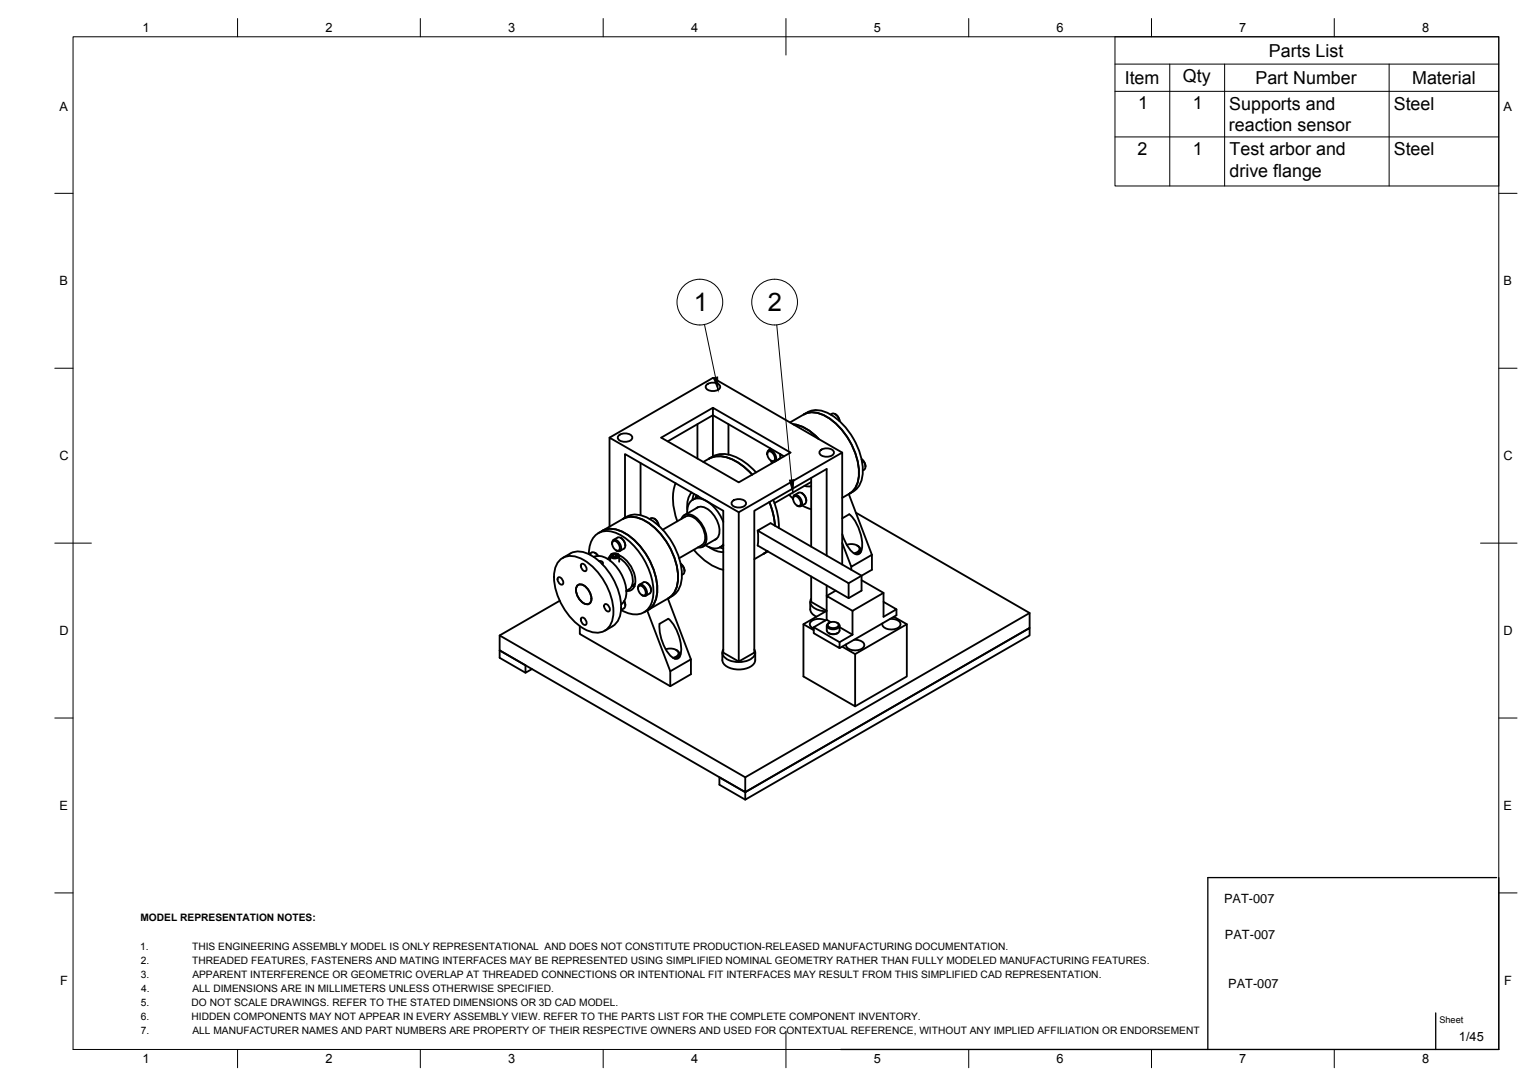
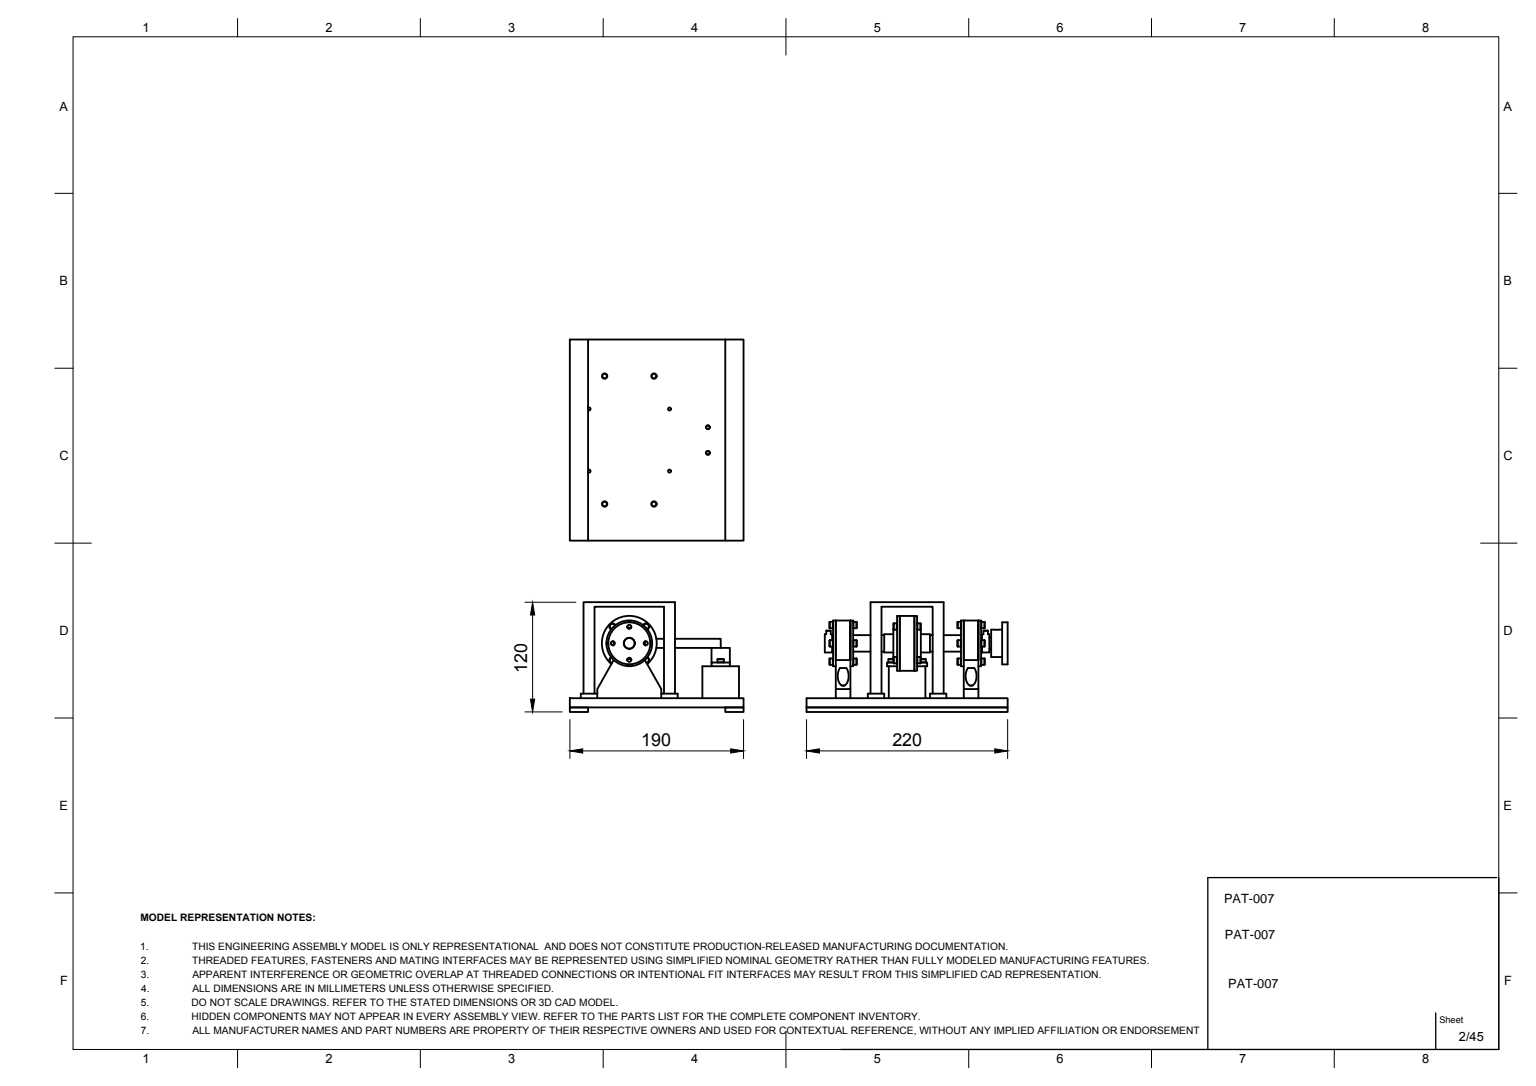
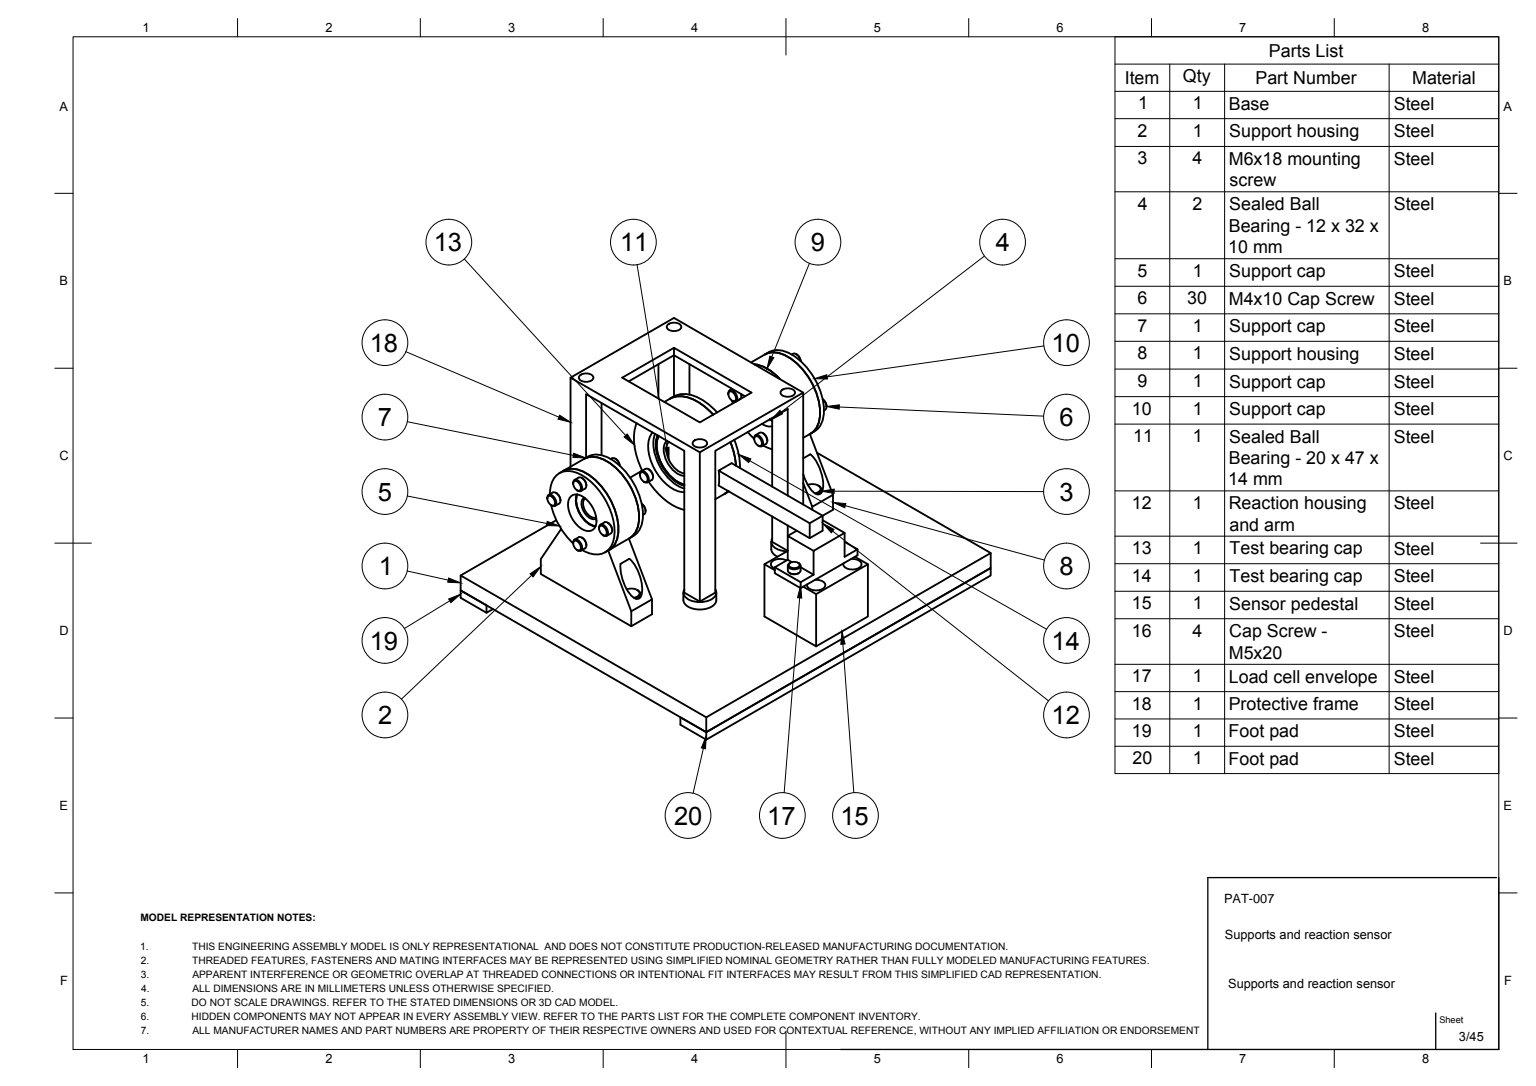
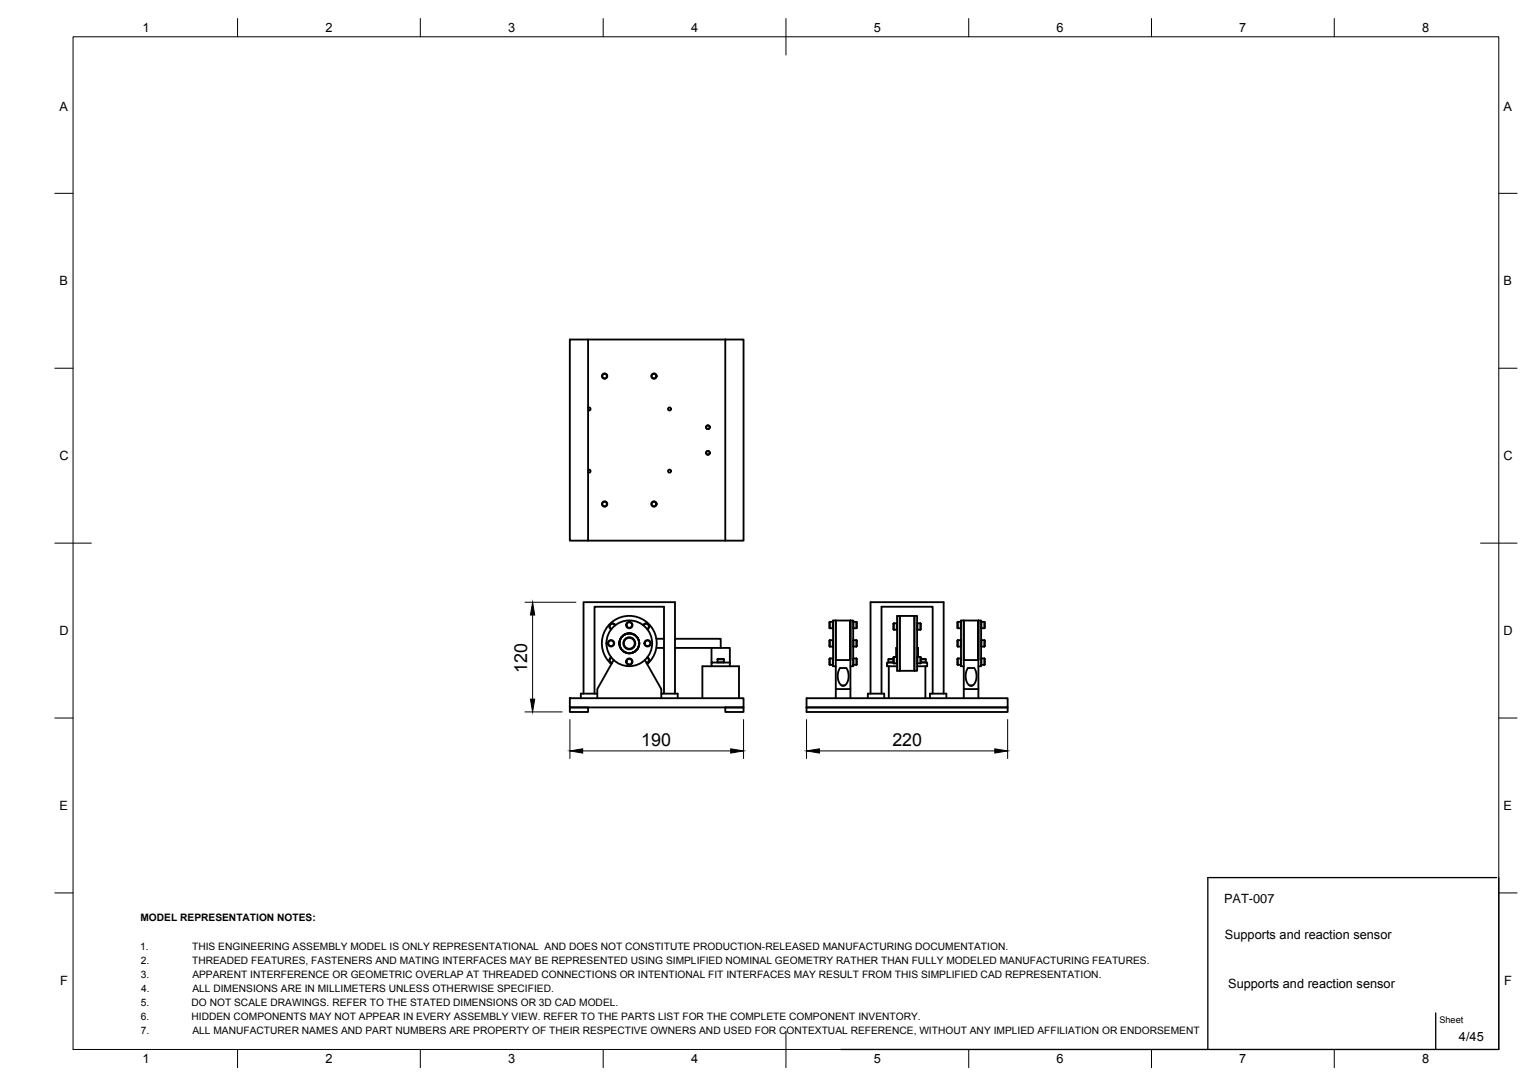
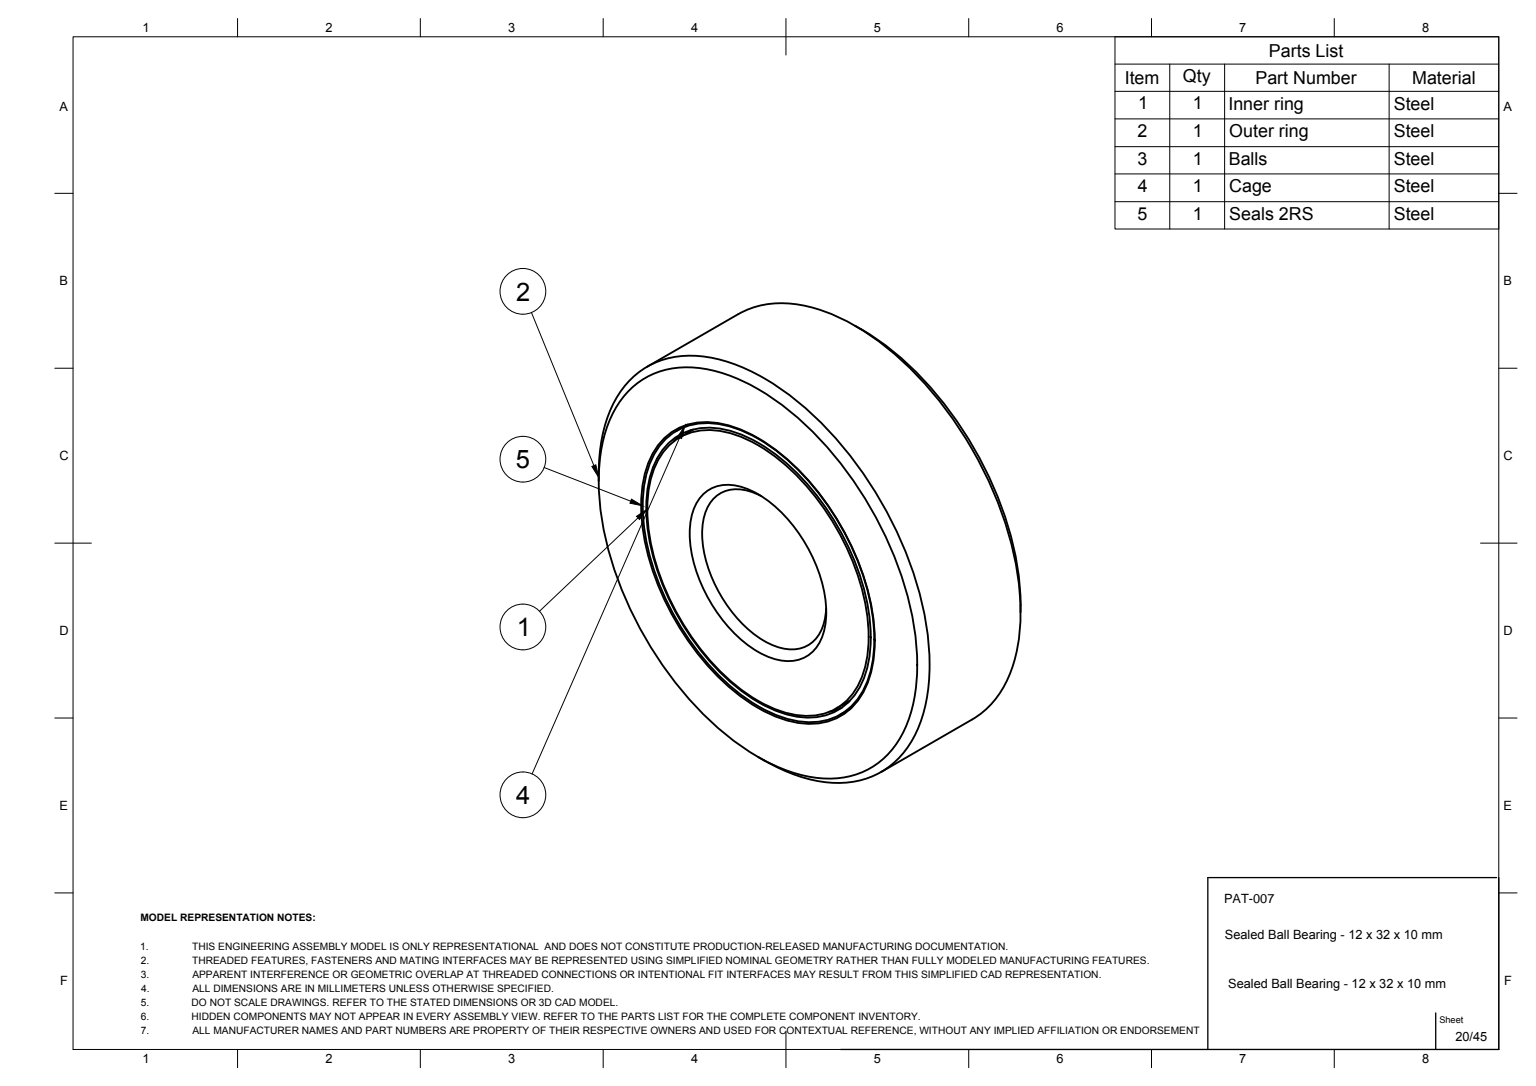
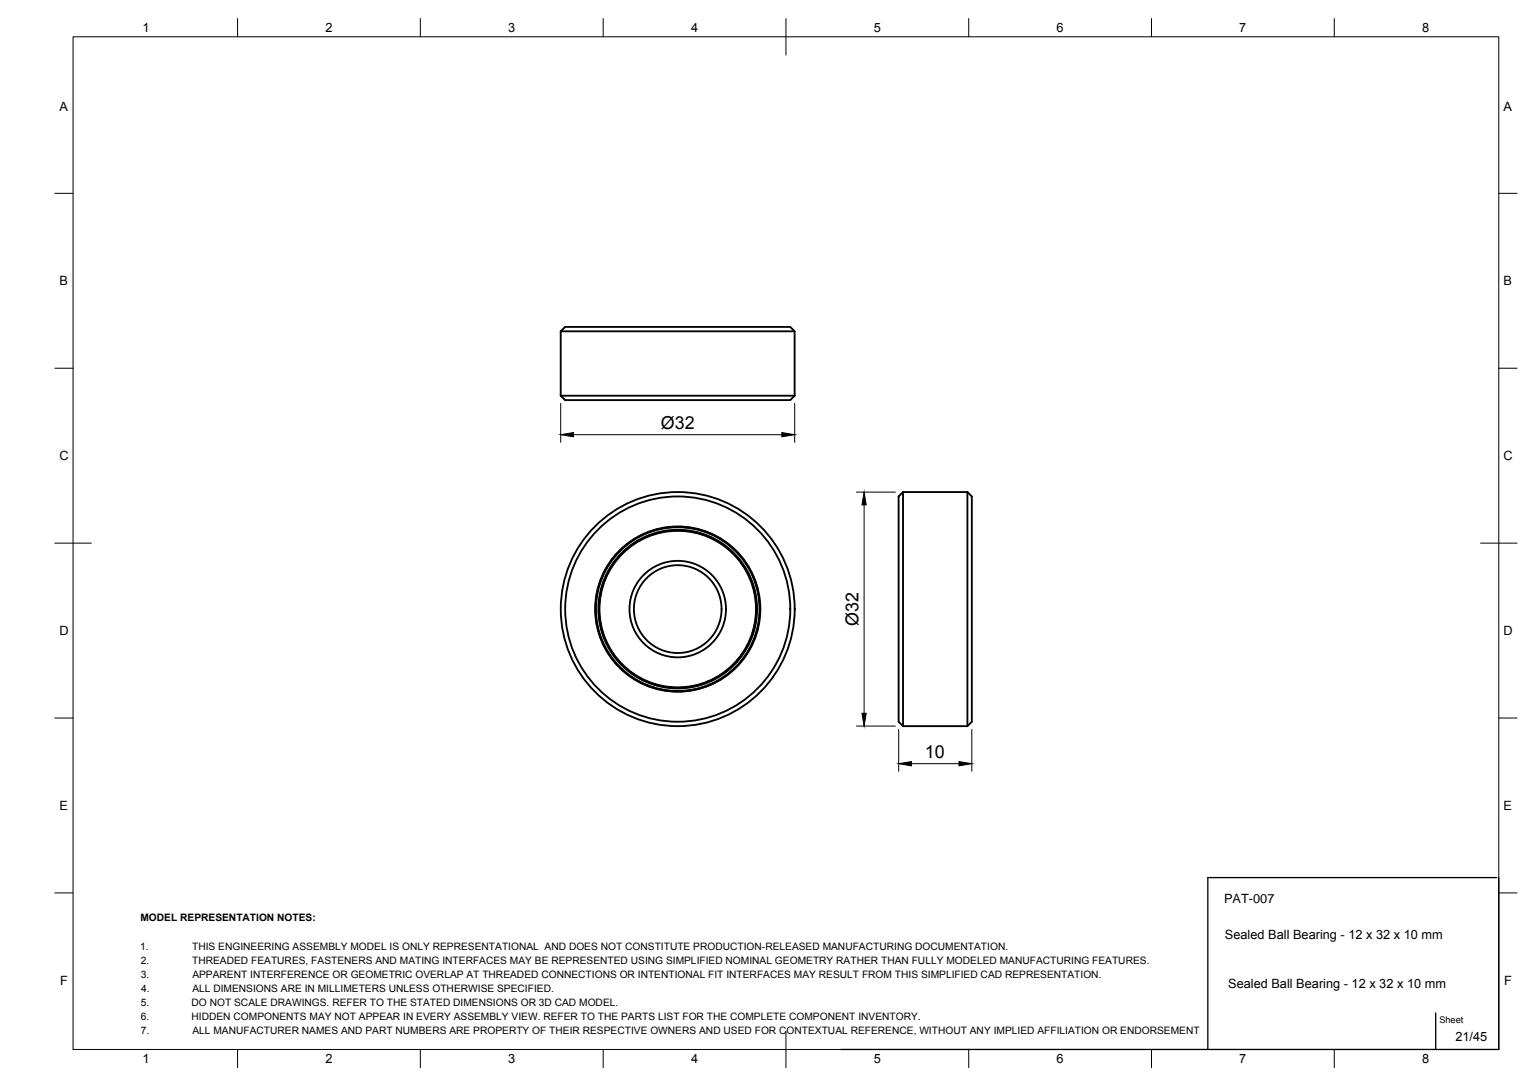
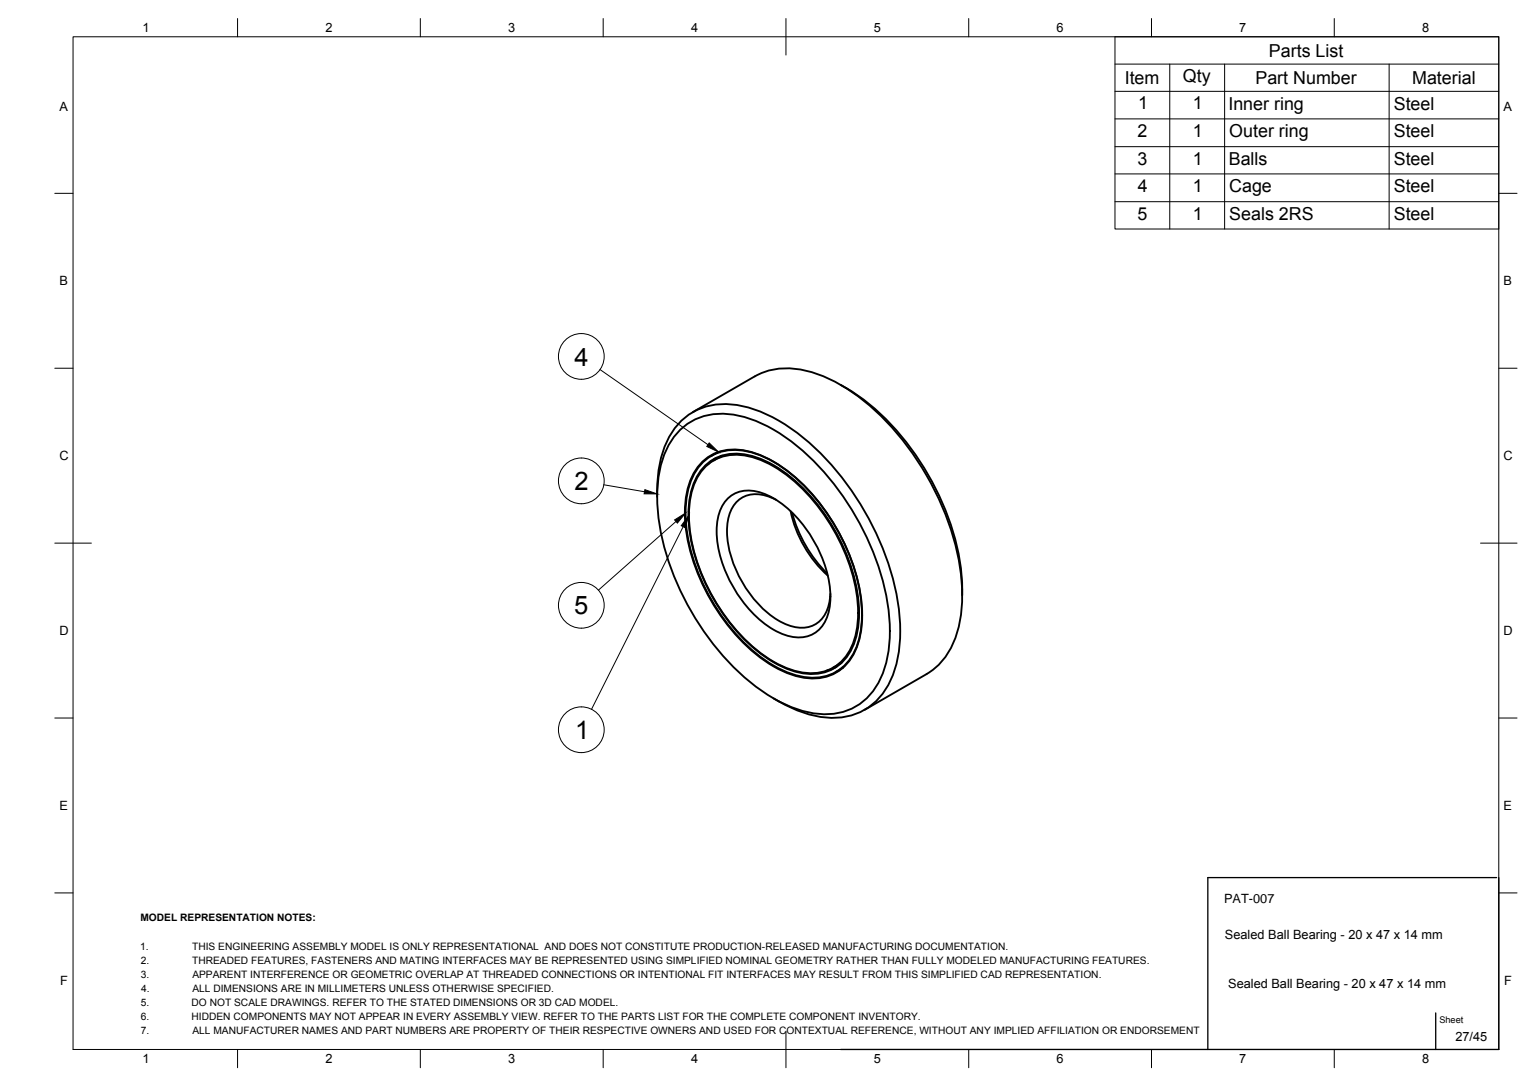
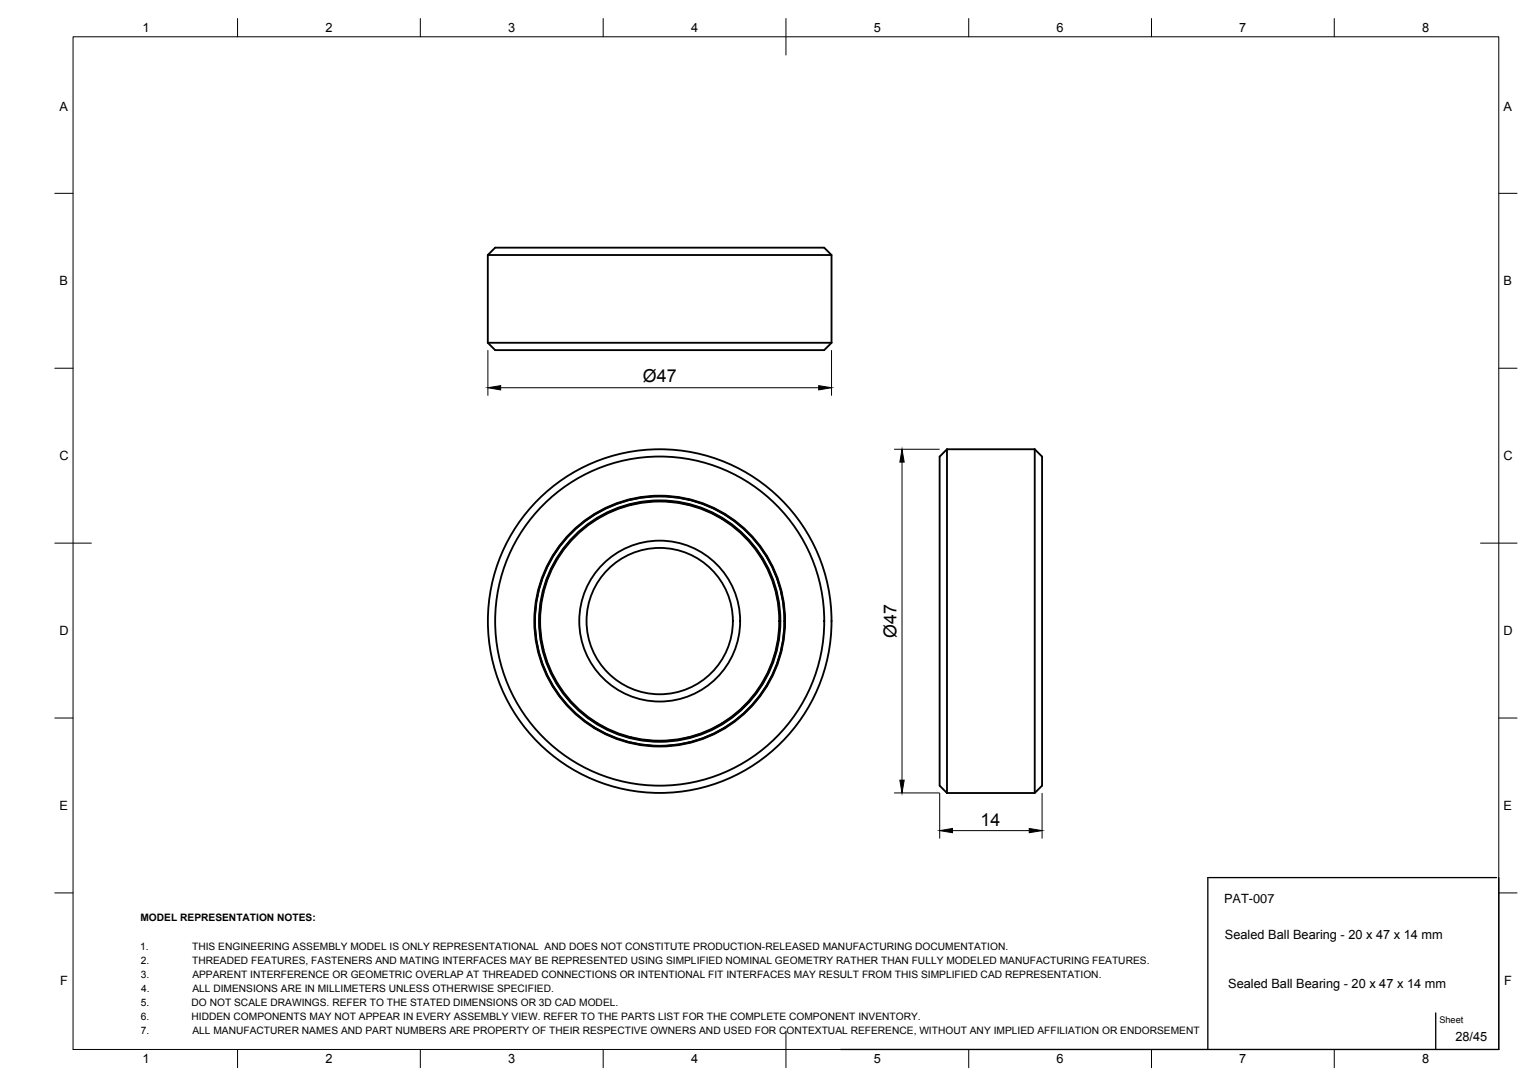
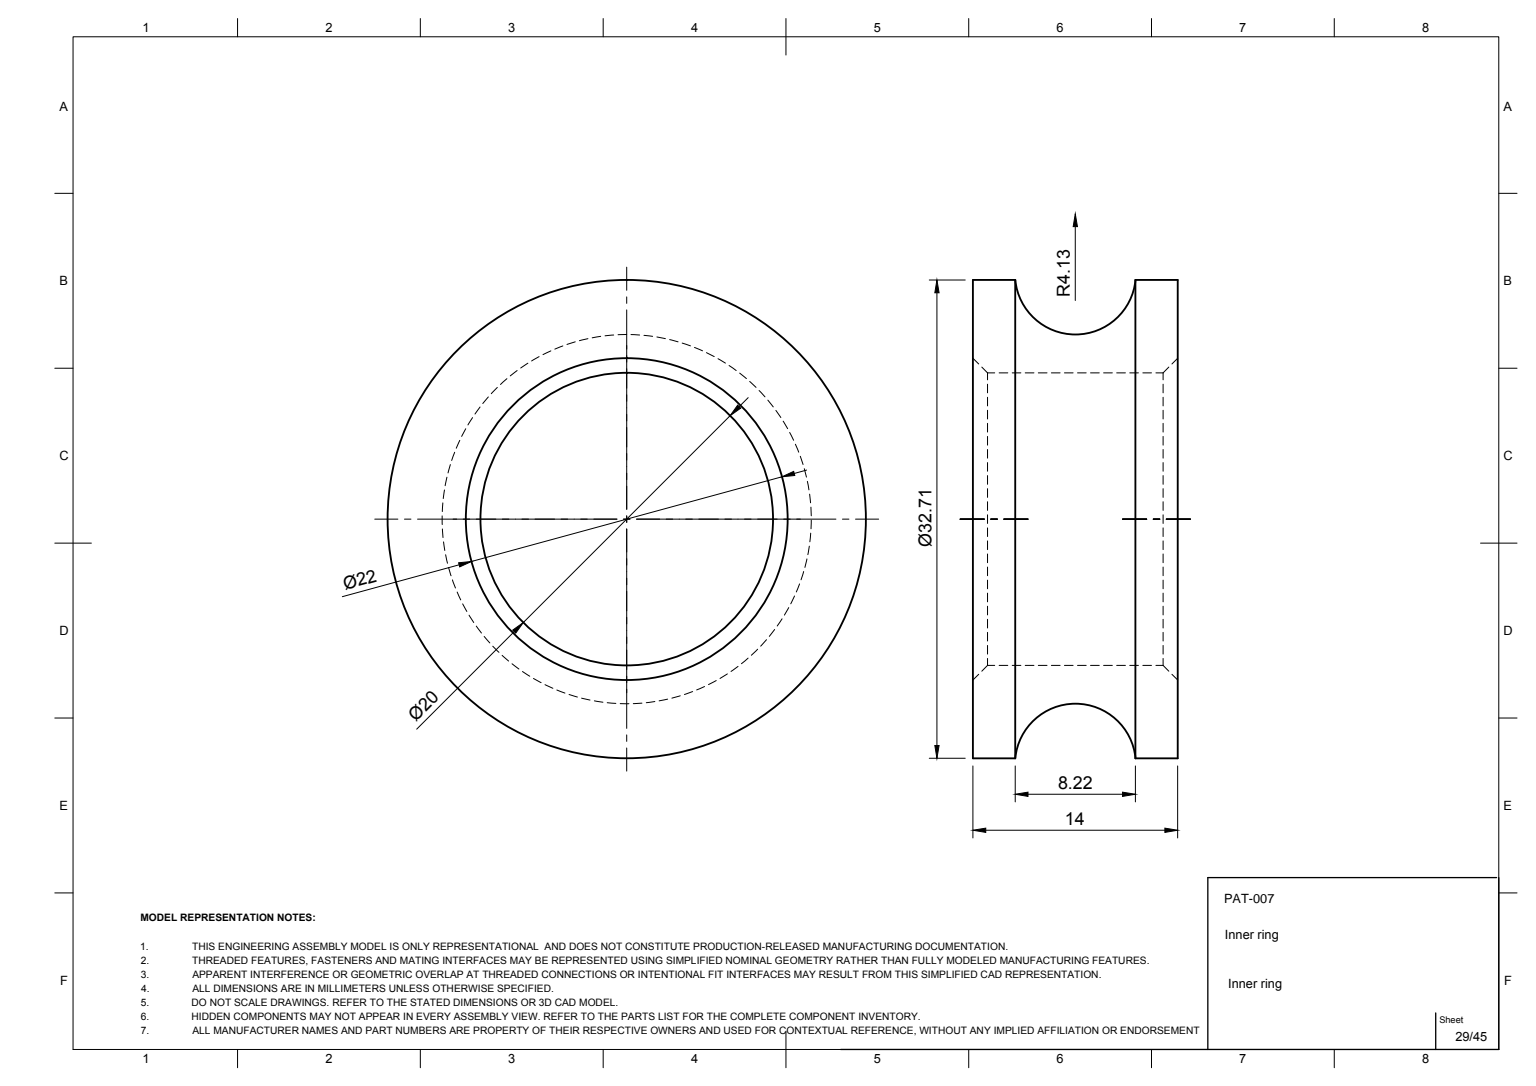
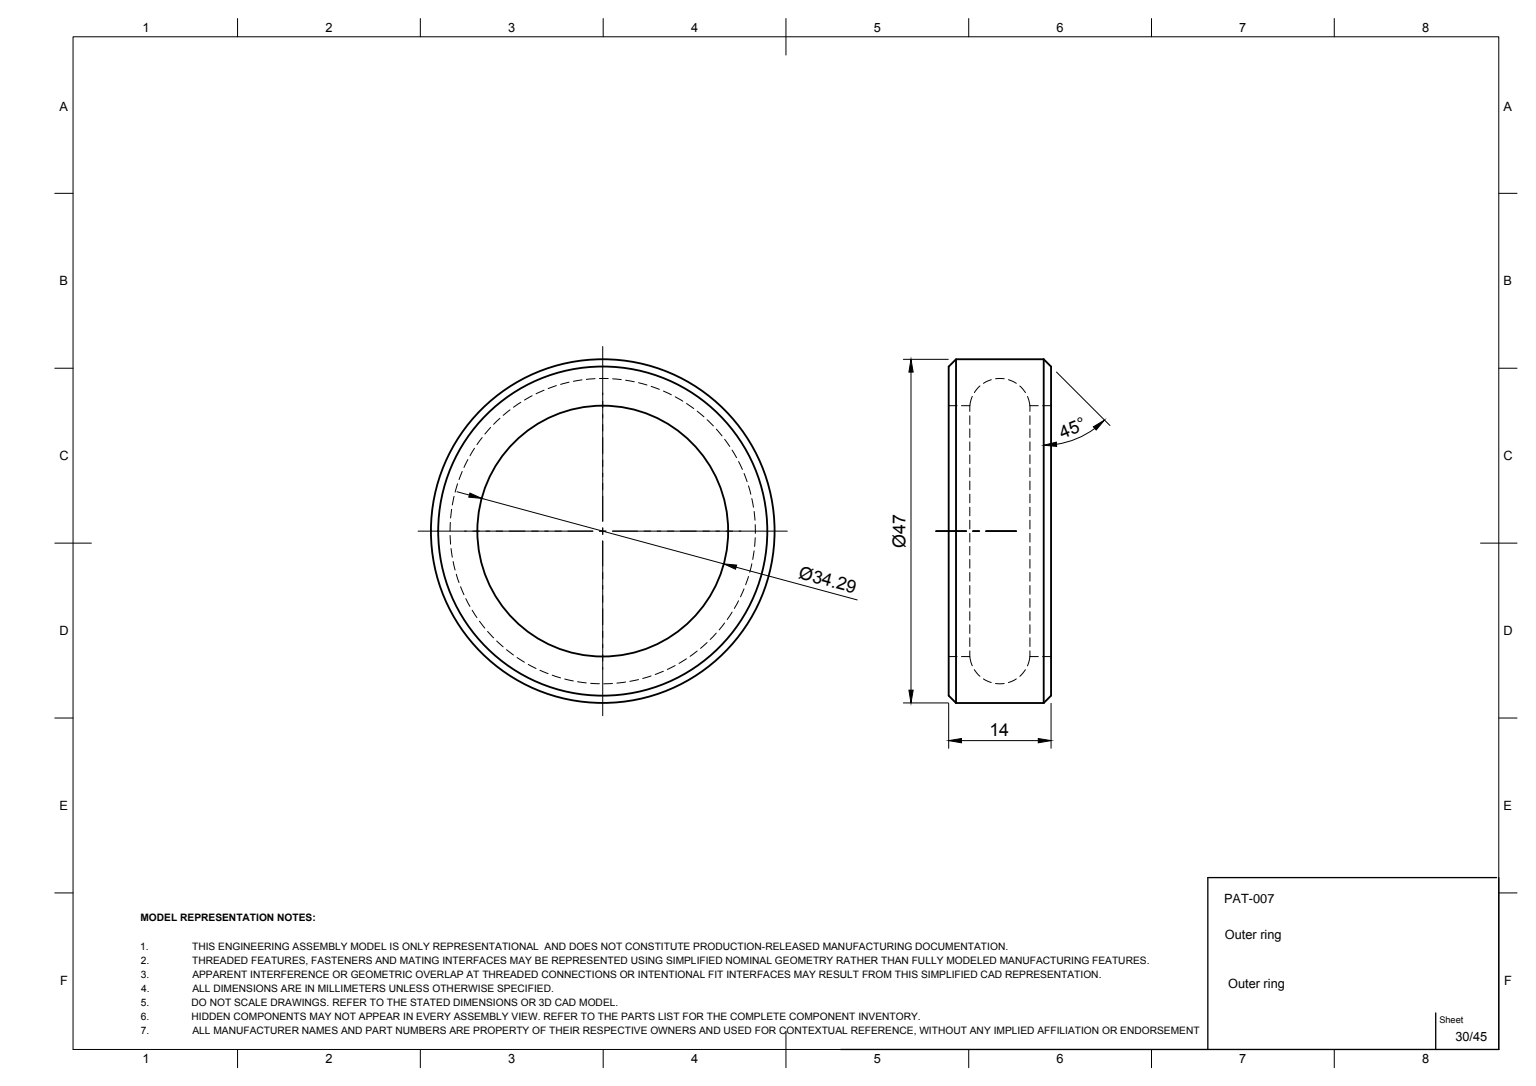
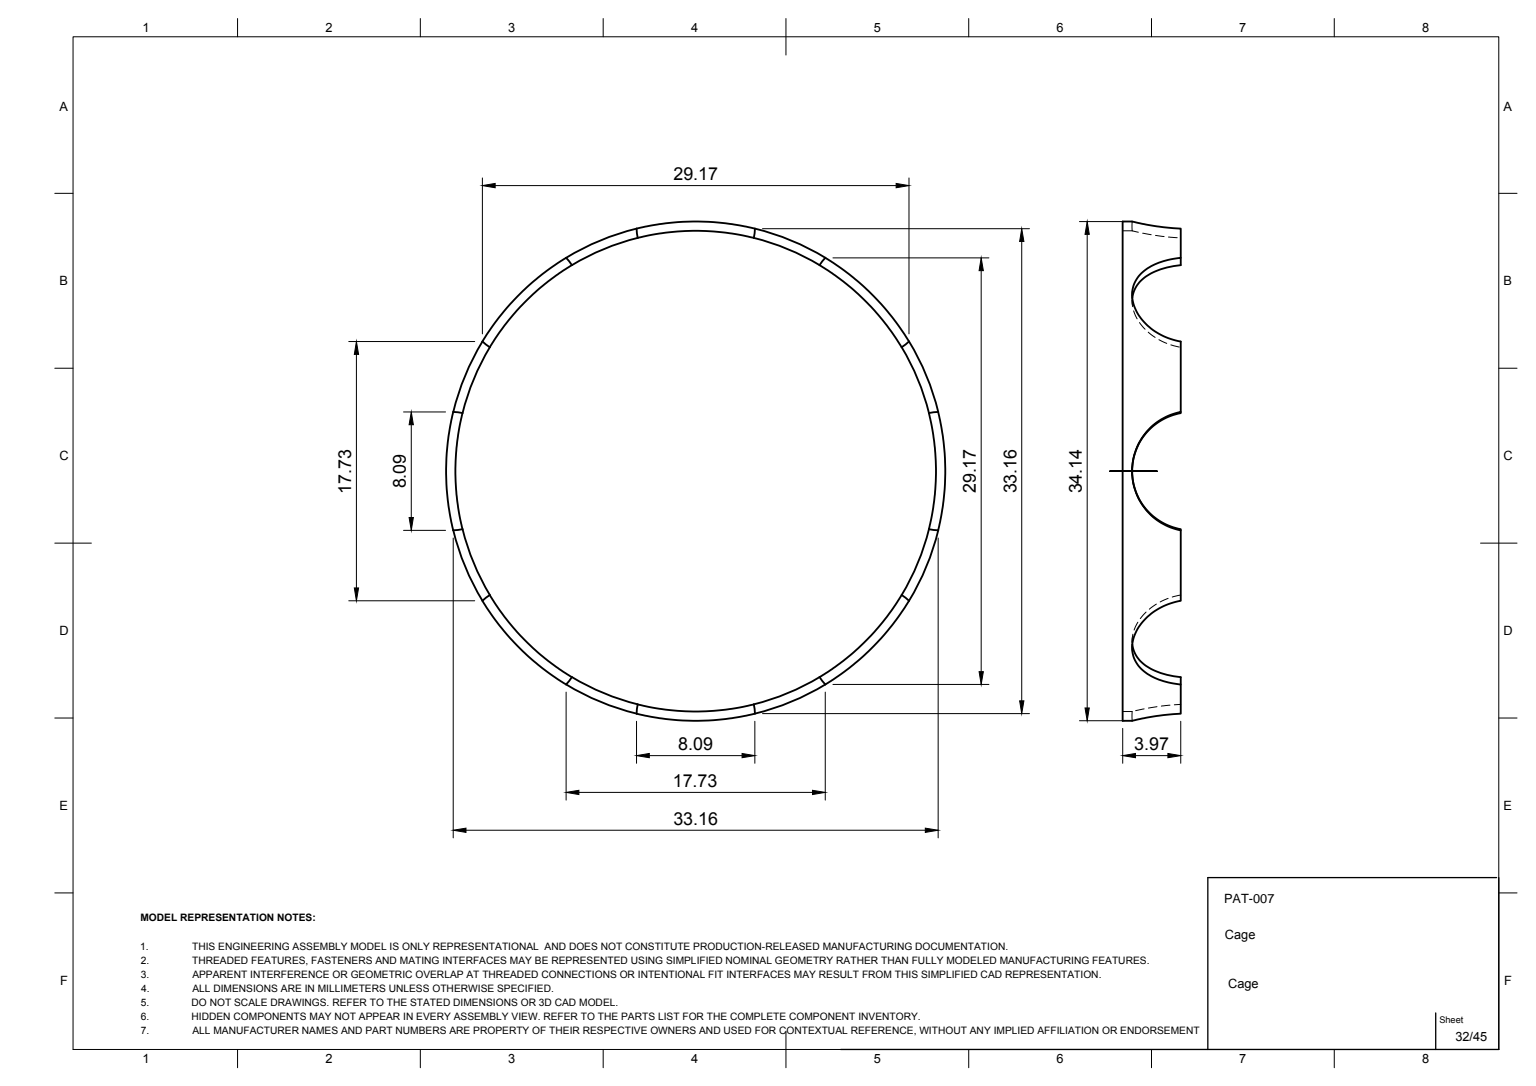
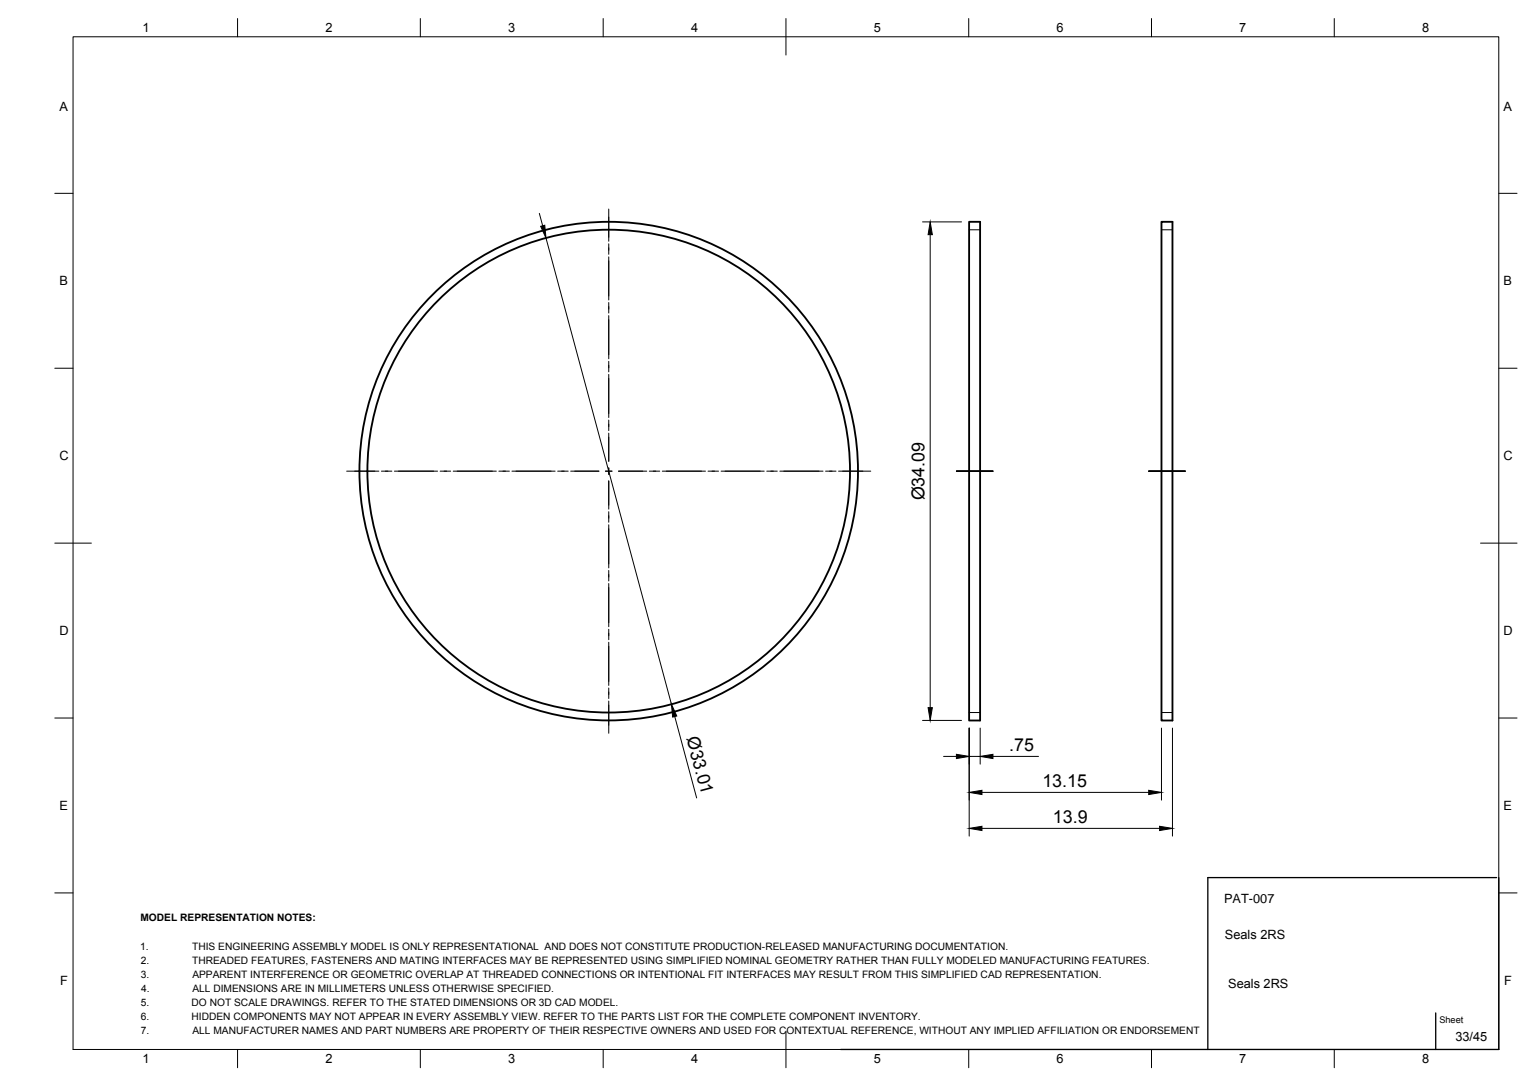
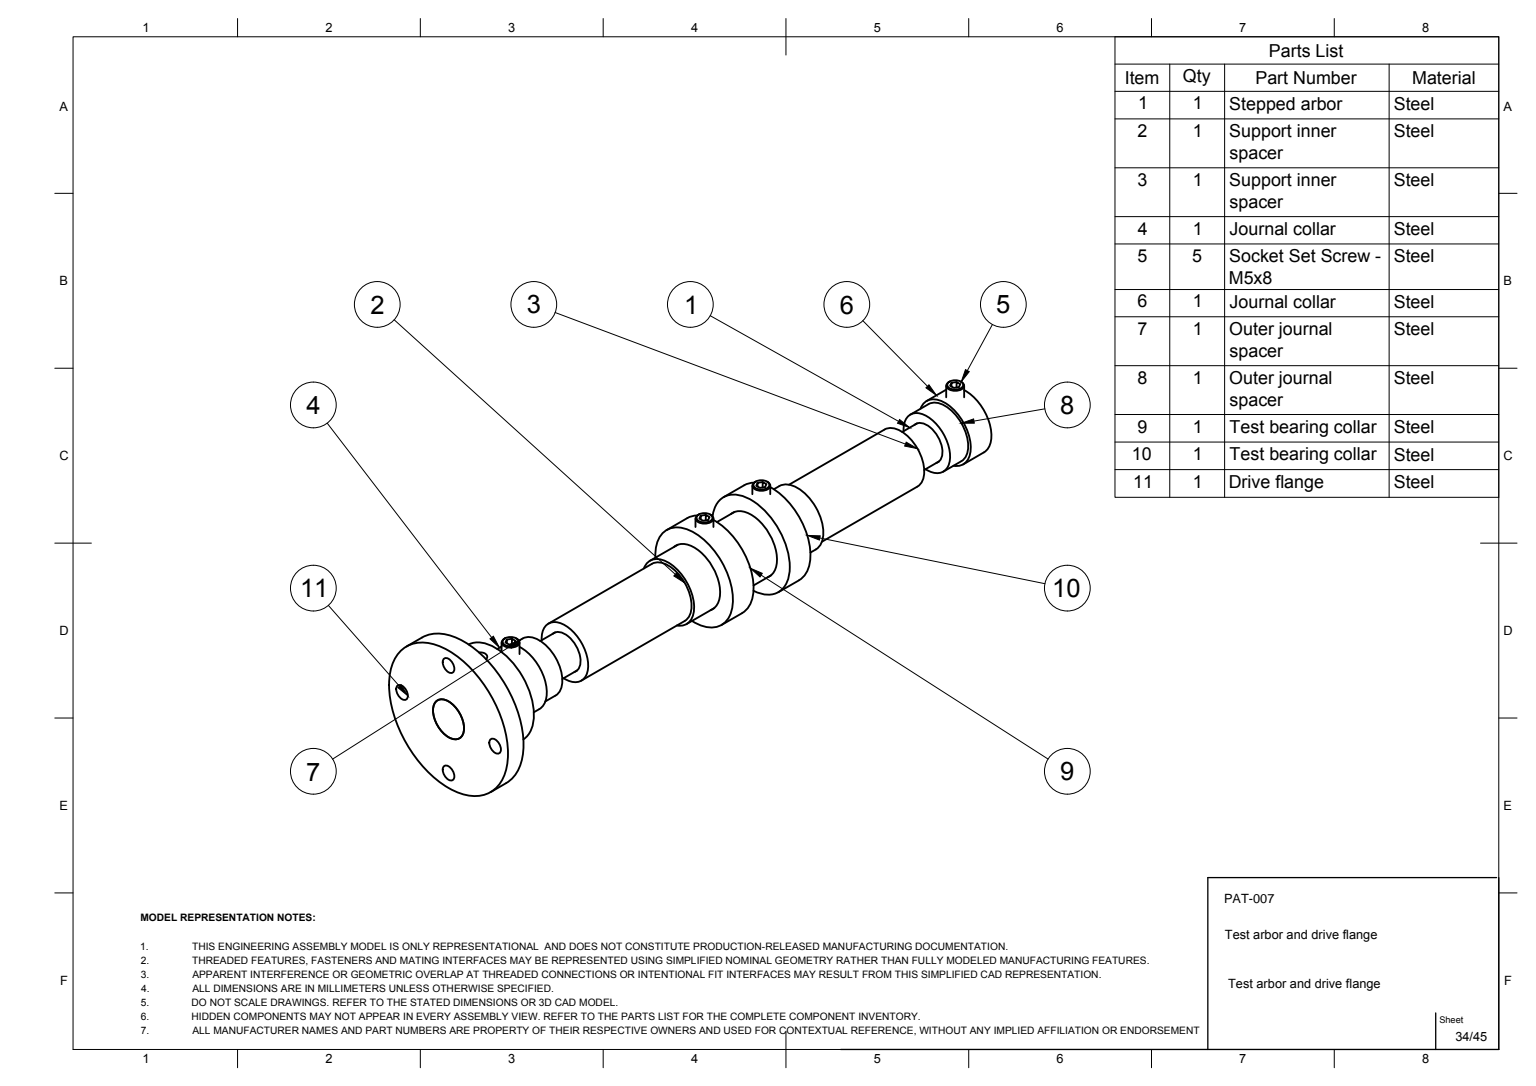
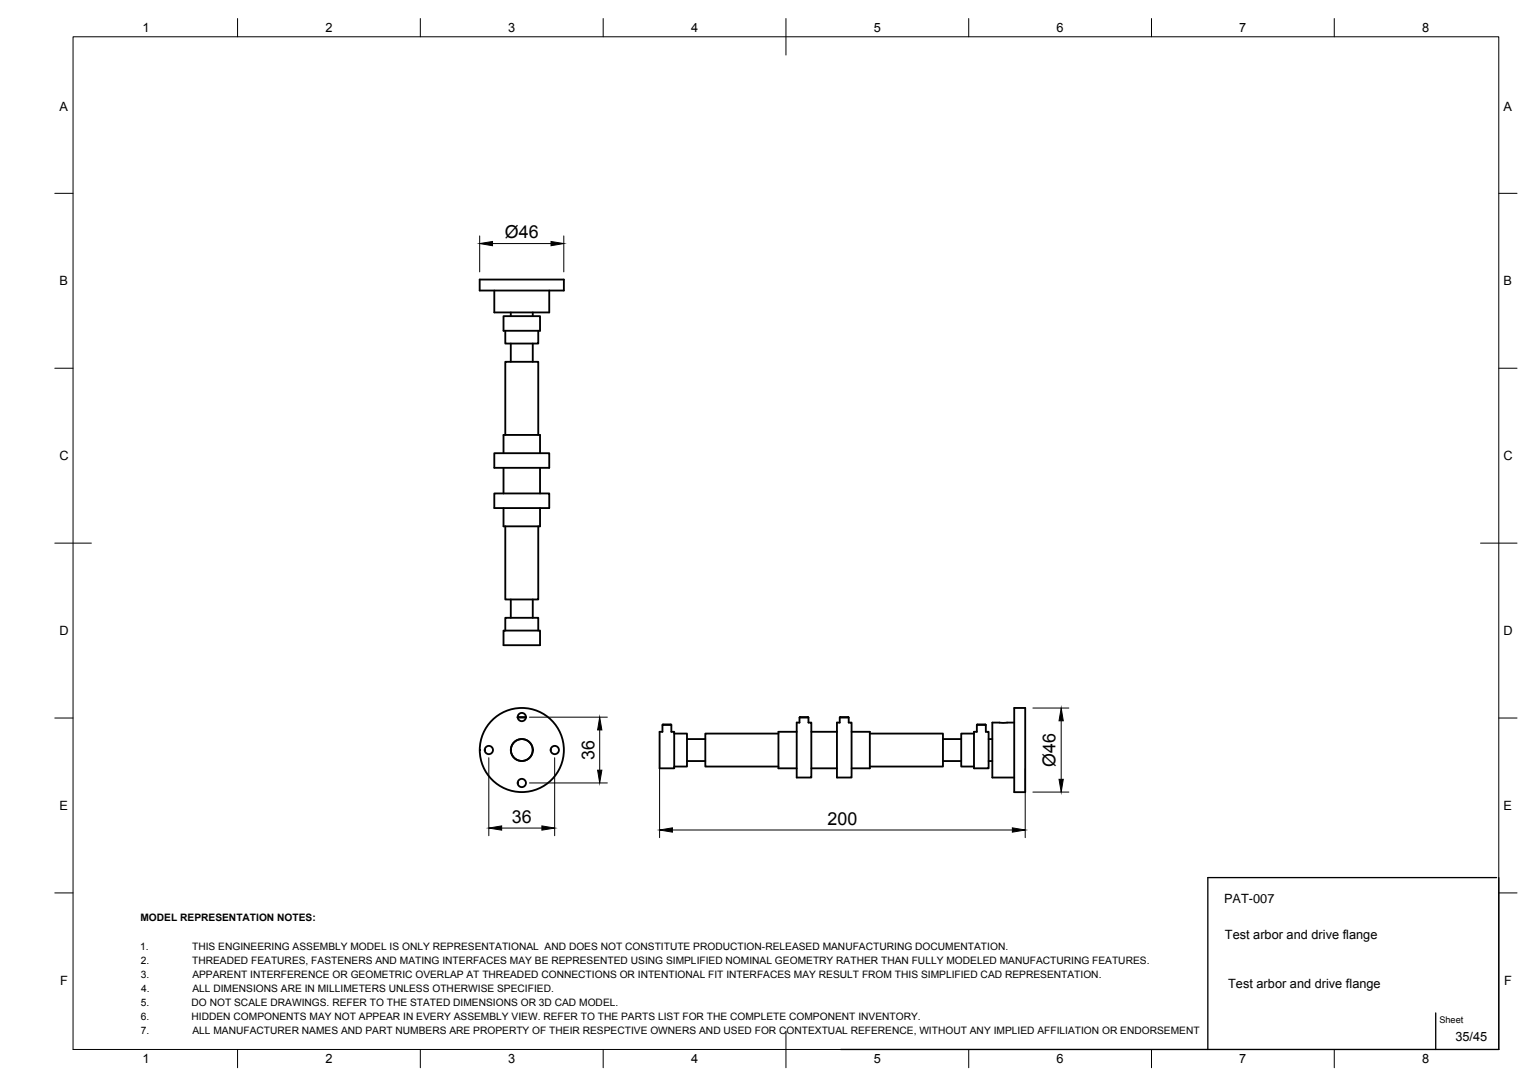
ISO-10303-21;
HEADER;
/* Generated by software containing ST-Developer
 * from STEP Tools, Inc. (www.steptools.com) 
 */

FILE_DESCRIPTION(
/* description */ ('Bearing friction torque test rig'),
/* implementation_level */ '2;1');

FILE_NAME(
/* name */ 'PAT-007',
/* time_stamp */ '2026-10-28T03:24:04-07:00',
/* author */ (''),
/* organization */ (''),
/* preprocessor_version */ 'ST-DEVELOPER v20.2',
/* originating_system */ 'Autodesk Translation Framework v15.17.0.0',
/* authorisation */ '');

FILE_SCHEMA (('AUTOMOTIVE_DESIGN { 1 0 10303 214 3 1 1 }'));
ENDSEC;

DATA;
#10=MECHANICAL_DESIGN_GEOMETRIC_PRESENTATION_REPRESENTATION('',(#539,#540,
#541,#542,#543,#544,#545,#546,#547,#548,#549,#550,#551,#552,#553,#554,#555,
#556,#557,#558,#559,#560,#561,#562,#563,#564,#565,#566,#567,#568,#569,#570,
#571,#572,#573,#574,#575,#576,#577,#578,#579,#580,#581,#582,#583,#584,#585,
#586,#587,#588,#589,#590,#591,#592),#14822);
#11=ITEM_DEFINED_TRANSFORMATION($,$,#8623,#8745);
#12=ITEM_DEFINED_TRANSFORMATION($,$,#8643,#8746);
#13=ITEM_DEFINED_TRANSFORMATION($,$,#8663,#8747);
#14=ITEM_DEFINED_TRANSFORMATION($,$,#8678,#8748);
#15=ITEM_DEFINED_TRANSFORMATION($,$,#8728,#8749);
#16=ITEM_DEFINED_TRANSFORMATION($,$,#8751,#8879);
#17=ITEM_DEFINED_TRANSFORMATION($,$,#8771,#8880);
#18=ITEM_DEFINED_TRANSFORMATION($,$,#8791,#8881);
#19=ITEM_DEFINED_TRANSFORMATION($,$,#8808,#8882);
#20=ITEM_DEFINED_TRANSFORMATION($,$,#8862,#8883);
#21=ITEM_DEFINED_TRANSFORMATION($,$,#8144,#8934);
#22=ITEM_DEFINED_TRANSFORMATION($,$,#8187,#8935);
#23=ITEM_DEFINED_TRANSFORMATION($,$,#8233,#8936);
#24=ITEM_DEFINED_TRANSFORMATION($,$,#8258,#8937);
#25=ITEM_DEFINED_TRANSFORMATION($,$,#8283,#8938);
#26=ITEM_DEFINED_TRANSFORMATION($,$,#8329,#8939);
#27=ITEM_DEFINED_TRANSFORMATION($,$,#8354,#8940);
#28=ITEM_DEFINED_TRANSFORMATION($,$,#8379,#8941);
#29=ITEM_DEFINED_TRANSFORMATION($,$,#8407,#8942);
#30=ITEM_DEFINED_TRANSFORMATION($,$,#8432,#8943);
#31=ITEM_DEFINED_TRANSFORMATION($,$,#8457,#8944);
#32=ITEM_DEFINED_TRANSFORMATION($,$,#8500,#8945);
#33=ITEM_DEFINED_TRANSFORMATION($,$,#8517,#8946);
#34=ITEM_DEFINED_TRANSFORMATION($,$,#8584,#8947);
#35=ITEM_DEFINED_TRANSFORMATION($,$,#8591,#8948);
#36=ITEM_DEFINED_TRANSFORMATION($,$,#8598,#8949);
#37=ITEM_DEFINED_TRANSFORMATION($,$,#8598,#8950);
#38=ITEM_DEFINED_TRANSFORMATION($,$,#8622,#8951);
#39=ITEM_DEFINED_TRANSFORMATION($,$,#8910,#8952);
#40=ITEM_DEFINED_TRANSFORMATION($,$,#8910,#8953);
#41=ITEM_DEFINED_TRANSFORMATION($,$,#8910,#8954);
#42=ITEM_DEFINED_TRANSFORMATION($,$,#8910,#8955);
#43=ITEM_DEFINED_TRANSFORMATION($,$,#8910,#8956);
#44=ITEM_DEFINED_TRANSFORMATION($,$,#8910,#8957);
#45=ITEM_DEFINED_TRANSFORMATION($,$,#8910,#8958);
#46=ITEM_DEFINED_TRANSFORMATION($,$,#8910,#8959);
#47=ITEM_DEFINED_TRANSFORMATION($,$,#8598,#8960);
#48=ITEM_DEFINED_TRANSFORMATION($,$,#8598,#8961);
#49=ITEM_DEFINED_TRANSFORMATION($,$,#8622,#8962);
#50=ITEM_DEFINED_TRANSFORMATION($,$,#8910,#8963);
#51=ITEM_DEFINED_TRANSFORMATION($,$,#8910,#8964);
#52=ITEM_DEFINED_TRANSFORMATION($,$,#8910,#8965);
#53=ITEM_DEFINED_TRANSFORMATION($,$,#8910,#8966);
#54=ITEM_DEFINED_TRANSFORMATION($,$,#8910,#8967);
#55=ITEM_DEFINED_TRANSFORMATION($,$,#8910,#8968);
#56=ITEM_DEFINED_TRANSFORMATION($,$,#8910,#8969);
#57=ITEM_DEFINED_TRANSFORMATION($,$,#8910,#8970);
#58=ITEM_DEFINED_TRANSFORMATION($,$,#8750,#8971);
#59=ITEM_DEFINED_TRANSFORMATION($,$,#8910,#8972);
#60=ITEM_DEFINED_TRANSFORMATION($,$,#8910,#8973);
#61=ITEM_DEFINED_TRANSFORMATION($,$,#8910,#8974);
#62=ITEM_DEFINED_TRANSFORMATION($,$,#8910,#8975);
#63=ITEM_DEFINED_TRANSFORMATION($,$,#8910,#8976);
#64=ITEM_DEFINED_TRANSFORMATION($,$,#8910,#8977);
#65=ITEM_DEFINED_TRANSFORMATION($,$,#8910,#8978);
#66=ITEM_DEFINED_TRANSFORMATION($,$,#8910,#8979);
#67=ITEM_DEFINED_TRANSFORMATION($,$,#8884,#8980);
#68=ITEM_DEFINED_TRANSFORMATION($,$,#8884,#8981);
#69=ITEM_DEFINED_TRANSFORMATION($,$,#8884,#8982);
#70=ITEM_DEFINED_TRANSFORMATION($,$,#8884,#8983);
#71=ITEM_DEFINED_TRANSFORMATION($,$,#8910,#8984);
#72=ITEM_DEFINED_TRANSFORMATION($,$,#8910,#8985);
#73=ITEM_DEFINED_TRANSFORMATION($,$,#8910,#8986);
#74=ITEM_DEFINED_TRANSFORMATION($,$,#8910,#8987);
#75=ITEM_DEFINED_TRANSFORMATION($,$,#8910,#8988);
#76=ITEM_DEFINED_TRANSFORMATION($,$,#8910,#8989);
#77=ITEM_DEFINED_TRANSFORMATION($,$,#8991,#9149);
#78=ITEM_DEFINED_TRANSFORMATION($,$,#9005,#9150);
#79=ITEM_DEFINED_TRANSFORMATION($,$,#9014,#9151);
#80=ITEM_DEFINED_TRANSFORMATION($,$,#9023,#9152);
#81=ITEM_DEFINED_TRANSFORMATION($,$,#9038,#9153);
#82=ITEM_DEFINED_TRANSFORMATION($,$,#9053,#9154);
#83=ITEM_DEFINED_TRANSFORMATION($,$,#9062,#9155);
#84=ITEM_DEFINED_TRANSFORMATION($,$,#9071,#9156);
#85=ITEM_DEFINED_TRANSFORMATION($,$,#9086,#9157);
#86=ITEM_DEFINED_TRANSFORMATION($,$,#9101,#9158);
#87=ITEM_DEFINED_TRANSFORMATION($,$,#9132,#9159);
#88=ITEM_DEFINED_TRANSFORMATION($,$,#9132,#9160);
#89=ITEM_DEFINED_TRANSFORMATION($,$,#9132,#9161);
#90=ITEM_DEFINED_TRANSFORMATION($,$,#9132,#9162);
#91=ITEM_DEFINED_TRANSFORMATION($,$,#9132,#9163);
#92=ITEM_DEFINED_TRANSFORMATION($,$,#8143,#9164);
#93=ITEM_DEFINED_TRANSFORMATION($,$,#8990,#9165);
#94=(
REPRESENTATION_RELATIONSHIP($,$,#15017,#15016)
REPRESENTATION_RELATIONSHIP_WITH_TRANSFORMATION(#11)
SHAPE_REPRESENTATION_RELATIONSHIP()
);
#95=(
REPRESENTATION_RELATIONSHIP($,$,#15018,#15016)
REPRESENTATION_RELATIONSHIP_WITH_TRANSFORMATION(#12)
SHAPE_REPRESENTATION_RELATIONSHIP()
);
#96=(
REPRESENTATION_RELATIONSHIP($,$,#15019,#15016)
REPRESENTATION_RELATIONSHIP_WITH_TRANSFORMATION(#13)
SHAPE_REPRESENTATION_RELATIONSHIP()
);
#97=(
REPRESENTATION_RELATIONSHIP($,$,#15020,#15016)
REPRESENTATION_RELATIONSHIP_WITH_TRANSFORMATION(#14)
SHAPE_REPRESENTATION_RELATIONSHIP()
);
#98=(
REPRESENTATION_RELATIONSHIP($,$,#15021,#15016)
REPRESENTATION_RELATIONSHIP_WITH_TRANSFORMATION(#15)
SHAPE_REPRESENTATION_RELATIONSHIP()
);
#99=(
REPRESENTATION_RELATIONSHIP($,$,#15023,#15022)
REPRESENTATION_RELATIONSHIP_WITH_TRANSFORMATION(#16)
SHAPE_REPRESENTATION_RELATIONSHIP()
);
#100=(
REPRESENTATION_RELATIONSHIP($,$,#15024,#15022)
REPRESENTATION_RELATIONSHIP_WITH_TRANSFORMATION(#17)
SHAPE_REPRESENTATION_RELATIONSHIP()
);
#101=(
REPRESENTATION_RELATIONSHIP($,$,#15025,#15022)
REPRESENTATION_RELATIONSHIP_WITH_TRANSFORMATION(#18)
SHAPE_REPRESENTATION_RELATIONSHIP()
);
#102=(
REPRESENTATION_RELATIONSHIP($,$,#15026,#15022)
REPRESENTATION_RELATIONSHIP_WITH_TRANSFORMATION(#19)
SHAPE_REPRESENTATION_RELATIONSHIP()
);
#103=(
REPRESENTATION_RELATIONSHIP($,$,#15027,#15022)
REPRESENTATION_RELATIONSHIP_WITH_TRANSFORMATION(#20)
SHAPE_REPRESENTATION_RELATIONSHIP()
);
#104=(
REPRESENTATION_RELATIONSHIP($,$,#15000,#14999)
REPRESENTATION_RELATIONSHIP_WITH_TRANSFORMATION(#21)
SHAPE_REPRESENTATION_RELATIONSHIP()
);
#105=(
REPRESENTATION_RELATIONSHIP($,$,#15001,#14999)
REPRESENTATION_RELATIONSHIP_WITH_TRANSFORMATION(#22)
SHAPE_REPRESENTATION_RELATIONSHIP()
);
#106=(
REPRESENTATION_RELATIONSHIP($,$,#15002,#14999)
REPRESENTATION_RELATIONSHIP_WITH_TRANSFORMATION(#23)
SHAPE_REPRESENTATION_RELATIONSHIP()
);
#107=(
REPRESENTATION_RELATIONSHIP($,$,#15003,#14999)
REPRESENTATION_RELATIONSHIP_WITH_TRANSFORMATION(#24)
SHAPE_REPRESENTATION_RELATIONSHIP()
);
#108=(
REPRESENTATION_RELATIONSHIP($,$,#15004,#14999)
REPRESENTATION_RELATIONSHIP_WITH_TRANSFORMATION(#25)
SHAPE_REPRESENTATION_RELATIONSHIP()
);
#109=(
REPRESENTATION_RELATIONSHIP($,$,#15005,#14999)
REPRESENTATION_RELATIONSHIP_WITH_TRANSFORMATION(#26)
SHAPE_REPRESENTATION_RELATIONSHIP()
);
#110=(
REPRESENTATION_RELATIONSHIP($,$,#15006,#14999)
REPRESENTATION_RELATIONSHIP_WITH_TRANSFORMATION(#27)
SHAPE_REPRESENTATION_RELATIONSHIP()
);
#111=(
REPRESENTATION_RELATIONSHIP($,$,#15007,#14999)
REPRESENTATION_RELATIONSHIP_WITH_TRANSFORMATION(#28)
SHAPE_REPRESENTATION_RELATIONSHIP()
);
#112=(
REPRESENTATION_RELATIONSHIP($,$,#15008,#14999)
REPRESENTATION_RELATIONSHIP_WITH_TRANSFORMATION(#29)
SHAPE_REPRESENTATION_RELATIONSHIP()
);
#113=(
REPRESENTATION_RELATIONSHIP($,$,#15009,#14999)
REPRESENTATION_RELATIONSHIP_WITH_TRANSFORMATION(#30)
SHAPE_REPRESENTATION_RELATIONSHIP()
);
#114=(
REPRESENTATION_RELATIONSHIP($,$,#15010,#14999)
REPRESENTATION_RELATIONSHIP_WITH_TRANSFORMATION(#31)
SHAPE_REPRESENTATION_RELATIONSHIP()
);
#115=(
REPRESENTATION_RELATIONSHIP($,$,#15011,#14999)
REPRESENTATION_RELATIONSHIP_WITH_TRANSFORMATION(#32)
SHAPE_REPRESENTATION_RELATIONSHIP()
);
#116=(
REPRESENTATION_RELATIONSHIP($,$,#15012,#14999)
REPRESENTATION_RELATIONSHIP_WITH_TRANSFORMATION(#33)
SHAPE_REPRESENTATION_RELATIONSHIP()
);
#117=(
REPRESENTATION_RELATIONSHIP($,$,#15013,#14999)
REPRESENTATION_RELATIONSHIP_WITH_TRANSFORMATION(#34)
SHAPE_REPRESENTATION_RELATIONSHIP()
);
#118=(
REPRESENTATION_RELATIONSHIP($,$,#15014,#14999)
REPRESENTATION_RELATIONSHIP_WITH_TRANSFORMATION(#35)
SHAPE_REPRESENTATION_RELATIONSHIP()
);
#119=(
REPRESENTATION_RELATIONSHIP($,$,#15015,#14999)
REPRESENTATION_RELATIONSHIP_WITH_TRANSFORMATION(#36)
SHAPE_REPRESENTATION_RELATIONSHIP()
);
#120=(
REPRESENTATION_RELATIONSHIP($,$,#15015,#14999)
REPRESENTATION_RELATIONSHIP_WITH_TRANSFORMATION(#37)
SHAPE_REPRESENTATION_RELATIONSHIP()
);
#121=(
REPRESENTATION_RELATIONSHIP($,$,#15016,#14999)
REPRESENTATION_RELATIONSHIP_WITH_TRANSFORMATION(#38)
SHAPE_REPRESENTATION_RELATIONSHIP()
);
#122=(
REPRESENTATION_RELATIONSHIP($,$,#15029,#14999)
REPRESENTATION_RELATIONSHIP_WITH_TRANSFORMATION(#39)
SHAPE_REPRESENTATION_RELATIONSHIP()
);
#123=(
REPRESENTATION_RELATIONSHIP($,$,#15029,#14999)
REPRESENTATION_RELATIONSHIP_WITH_TRANSFORMATION(#40)
SHAPE_REPRESENTATION_RELATIONSHIP()
);
#124=(
REPRESENTATION_RELATIONSHIP($,$,#15029,#14999)
REPRESENTATION_RELATIONSHIP_WITH_TRANSFORMATION(#41)
SHAPE_REPRESENTATION_RELATIONSHIP()
);
#125=(
REPRESENTATION_RELATIONSHIP($,$,#15029,#14999)
REPRESENTATION_RELATIONSHIP_WITH_TRANSFORMATION(#42)
SHAPE_REPRESENTATION_RELATIONSHIP()
);
#126=(
REPRESENTATION_RELATIONSHIP($,$,#15029,#14999)
REPRESENTATION_RELATIONSHIP_WITH_TRANSFORMATION(#43)
SHAPE_REPRESENTATION_RELATIONSHIP()
);
#127=(
REPRESENTATION_RELATIONSHIP($,$,#15029,#14999)
REPRESENTATION_RELATIONSHIP_WITH_TRANSFORMATION(#44)
SHAPE_REPRESENTATION_RELATIONSHIP()
);
#128=(
REPRESENTATION_RELATIONSHIP($,$,#15029,#14999)
REPRESENTATION_RELATIONSHIP_WITH_TRANSFORMATION(#45)
SHAPE_REPRESENTATION_RELATIONSHIP()
);
#129=(
REPRESENTATION_RELATIONSHIP($,$,#15029,#14999)
REPRESENTATION_RELATIONSHIP_WITH_TRANSFORMATION(#46)
SHAPE_REPRESENTATION_RELATIONSHIP()
);
#130=(
REPRESENTATION_RELATIONSHIP($,$,#15015,#14999)
REPRESENTATION_RELATIONSHIP_WITH_TRANSFORMATION(#47)
SHAPE_REPRESENTATION_RELATIONSHIP()
);
#131=(
REPRESENTATION_RELATIONSHIP($,$,#15015,#14999)
REPRESENTATION_RELATIONSHIP_WITH_TRANSFORMATION(#48)
SHAPE_REPRESENTATION_RELATIONSHIP()
);
#132=(
REPRESENTATION_RELATIONSHIP($,$,#15016,#14999)
REPRESENTATION_RELATIONSHIP_WITH_TRANSFORMATION(#49)
SHAPE_REPRESENTATION_RELATIONSHIP()
);
#133=(
REPRESENTATION_RELATIONSHIP($,$,#15029,#14999)
REPRESENTATION_RELATIONSHIP_WITH_TRANSFORMATION(#50)
SHAPE_REPRESENTATION_RELATIONSHIP()
);
#134=(
REPRESENTATION_RELATIONSHIP($,$,#15029,#14999)
REPRESENTATION_RELATIONSHIP_WITH_TRANSFORMATION(#51)
SHAPE_REPRESENTATION_RELATIONSHIP()
);
#135=(
REPRESENTATION_RELATIONSHIP($,$,#15029,#14999)
REPRESENTATION_RELATIONSHIP_WITH_TRANSFORMATION(#52)
SHAPE_REPRESENTATION_RELATIONSHIP()
);
#136=(
REPRESENTATION_RELATIONSHIP($,$,#15029,#14999)
REPRESENTATION_RELATIONSHIP_WITH_TRANSFORMATION(#53)
SHAPE_REPRESENTATION_RELATIONSHIP()
);
#137=(
REPRESENTATION_RELATIONSHIP($,$,#15029,#14999)
REPRESENTATION_RELATIONSHIP_WITH_TRANSFORMATION(#54)
SHAPE_REPRESENTATION_RELATIONSHIP()
);
#138=(
REPRESENTATION_RELATIONSHIP($,$,#15029,#14999)
REPRESENTATION_RELATIONSHIP_WITH_TRANSFORMATION(#55)
SHAPE_REPRESENTATION_RELATIONSHIP()
);
#139=(
REPRESENTATION_RELATIONSHIP($,$,#15029,#14999)
REPRESENTATION_RELATIONSHIP_WITH_TRANSFORMATION(#56)
SHAPE_REPRESENTATION_RELATIONSHIP()
);
#140=(
REPRESENTATION_RELATIONSHIP($,$,#15029,#14999)
REPRESENTATION_RELATIONSHIP_WITH_TRANSFORMATION(#57)
SHAPE_REPRESENTATION_RELATIONSHIP()
);
#141=(
REPRESENTATION_RELATIONSHIP($,$,#15022,#14999)
REPRESENTATION_RELATIONSHIP_WITH_TRANSFORMATION(#58)
SHAPE_REPRESENTATION_RELATIONSHIP()
);
#142=(
REPRESENTATION_RELATIONSHIP($,$,#15029,#14999)
REPRESENTATION_RELATIONSHIP_WITH_TRANSFORMATION(#59)
SHAPE_REPRESENTATION_RELATIONSHIP()
);
#143=(
REPRESENTATION_RELATIONSHIP($,$,#15029,#14999)
REPRESENTATION_RELATIONSHIP_WITH_TRANSFORMATION(#60)
SHAPE_REPRESENTATION_RELATIONSHIP()
);
#144=(
REPRESENTATION_RELATIONSHIP($,$,#15029,#14999)
REPRESENTATION_RELATIONSHIP_WITH_TRANSFORMATION(#61)
SHAPE_REPRESENTATION_RELATIONSHIP()
);
#145=(
REPRESENTATION_RELATIONSHIP($,$,#15029,#14999)
REPRESENTATION_RELATIONSHIP_WITH_TRANSFORMATION(#62)
SHAPE_REPRESENTATION_RELATIONSHIP()
);
#146=(
REPRESENTATION_RELATIONSHIP($,$,#15029,#14999)
REPRESENTATION_RELATIONSHIP_WITH_TRANSFORMATION(#63)
SHAPE_REPRESENTATION_RELATIONSHIP()
);
#147=(
REPRESENTATION_RELATIONSHIP($,$,#15029,#14999)
REPRESENTATION_RELATIONSHIP_WITH_TRANSFORMATION(#64)
SHAPE_REPRESENTATION_RELATIONSHIP()
);
#148=(
REPRESENTATION_RELATIONSHIP($,$,#15029,#14999)
REPRESENTATION_RELATIONSHIP_WITH_TRANSFORMATION(#65)
SHAPE_REPRESENTATION_RELATIONSHIP()
);
#149=(
REPRESENTATION_RELATIONSHIP($,$,#15029,#14999)
REPRESENTATION_RELATIONSHIP_WITH_TRANSFORMATION(#66)
SHAPE_REPRESENTATION_RELATIONSHIP()
);
#150=(
REPRESENTATION_RELATIONSHIP($,$,#15028,#14999)
REPRESENTATION_RELATIONSHIP_WITH_TRANSFORMATION(#67)
SHAPE_REPRESENTATION_RELATIONSHIP()
);
#151=(
REPRESENTATION_RELATIONSHIP($,$,#15028,#14999)
REPRESENTATION_RELATIONSHIP_WITH_TRANSFORMATION(#68)
SHAPE_REPRESENTATION_RELATIONSHIP()
);
#152=(
REPRESENTATION_RELATIONSHIP($,$,#15028,#14999)
REPRESENTATION_RELATIONSHIP_WITH_TRANSFORMATION(#69)
SHAPE_REPRESENTATION_RELATIONSHIP()
);
#153=(
REPRESENTATION_RELATIONSHIP($,$,#15028,#14999)
REPRESENTATION_RELATIONSHIP_WITH_TRANSFORMATION(#70)
SHAPE_REPRESENTATION_RELATIONSHIP()
);
#154=(
REPRESENTATION_RELATIONSHIP($,$,#15029,#14999)
REPRESENTATION_RELATIONSHIP_WITH_TRANSFORMATION(#71)
SHAPE_REPRESENTATION_RELATIONSHIP()
);
#155=(
REPRESENTATION_RELATIONSHIP($,$,#15029,#14999)
REPRESENTATION_RELATIONSHIP_WITH_TRANSFORMATION(#72)
SHAPE_REPRESENTATION_RELATIONSHIP()
);
#156=(
REPRESENTATION_RELATIONSHIP($,$,#15029,#14999)
REPRESENTATION_RELATIONSHIP_WITH_TRANSFORMATION(#73)
SHAPE_REPRESENTATION_RELATIONSHIP()
);
#157=(
REPRESENTATION_RELATIONSHIP($,$,#15029,#14999)
REPRESENTATION_RELATIONSHIP_WITH_TRANSFORMATION(#74)
SHAPE_REPRESENTATION_RELATIONSHIP()
);
#158=(
REPRESENTATION_RELATIONSHIP($,$,#15029,#14999)
REPRESENTATION_RELATIONSHIP_WITH_TRANSFORMATION(#75)
SHAPE_REPRESENTATION_RELATIONSHIP()
);
#159=(
REPRESENTATION_RELATIONSHIP($,$,#15029,#14999)
REPRESENTATION_RELATIONSHIP_WITH_TRANSFORMATION(#76)
SHAPE_REPRESENTATION_RELATIONSHIP()
);
#160=(
REPRESENTATION_RELATIONSHIP($,$,#15031,#15030)
REPRESENTATION_RELATIONSHIP_WITH_TRANSFORMATION(#77)
SHAPE_REPRESENTATION_RELATIONSHIP()
);
#161=(
REPRESENTATION_RELATIONSHIP($,$,#15032,#15030)
REPRESENTATION_RELATIONSHIP_WITH_TRANSFORMATION(#78)
SHAPE_REPRESENTATION_RELATIONSHIP()
);
#162=(
REPRESENTATION_RELATIONSHIP($,$,#15033,#15030)
REPRESENTATION_RELATIONSHIP_WITH_TRANSFORMATION(#79)
SHAPE_REPRESENTATION_RELATIONSHIP()
);
#163=(
REPRESENTATION_RELATIONSHIP($,$,#15034,#15030)
REPRESENTATION_RELATIONSHIP_WITH_TRANSFORMATION(#80)
SHAPE_REPRESENTATION_RELATIONSHIP()
);
#164=(
REPRESENTATION_RELATIONSHIP($,$,#15035,#15030)
REPRESENTATION_RELATIONSHIP_WITH_TRANSFORMATION(#81)
SHAPE_REPRESENTATION_RELATIONSHIP()
);
#165=(
REPRESENTATION_RELATIONSHIP($,$,#15036,#15030)
REPRESENTATION_RELATIONSHIP_WITH_TRANSFORMATION(#82)
SHAPE_REPRESENTATION_RELATIONSHIP()
);
#166=(
REPRESENTATION_RELATIONSHIP($,$,#15037,#15030)
REPRESENTATION_RELATIONSHIP_WITH_TRANSFORMATION(#83)
SHAPE_REPRESENTATION_RELATIONSHIP()
);
#167=(
REPRESENTATION_RELATIONSHIP($,$,#15038,#15030)
REPRESENTATION_RELATIONSHIP_WITH_TRANSFORMATION(#84)
SHAPE_REPRESENTATION_RELATIONSHIP()
);
#168=(
REPRESENTATION_RELATIONSHIP($,$,#15039,#15030)
REPRESENTATION_RELATIONSHIP_WITH_TRANSFORMATION(#85)
SHAPE_REPRESENTATION_RELATIONSHIP()
);
#169=(
REPRESENTATION_RELATIONSHIP($,$,#15040,#15030)
REPRESENTATION_RELATIONSHIP_WITH_TRANSFORMATION(#86)
SHAPE_REPRESENTATION_RELATIONSHIP()
);
#170=(
REPRESENTATION_RELATIONSHIP($,$,#15041,#15030)
REPRESENTATION_RELATIONSHIP_WITH_TRANSFORMATION(#87)
SHAPE_REPRESENTATION_RELATIONSHIP()
);
#171=(
REPRESENTATION_RELATIONSHIP($,$,#15041,#15030)
REPRESENTATION_RELATIONSHIP_WITH_TRANSFORMATION(#88)
SHAPE_REPRESENTATION_RELATIONSHIP()
);
#172=(
REPRESENTATION_RELATIONSHIP($,$,#15041,#15030)
REPRESENTATION_RELATIONSHIP_WITH_TRANSFORMATION(#89)
SHAPE_REPRESENTATION_RELATIONSHIP()
);
#173=(
REPRESENTATION_RELATIONSHIP($,$,#15041,#15030)
REPRESENTATION_RELATIONSHIP_WITH_TRANSFORMATION(#90)
SHAPE_REPRESENTATION_RELATIONSHIP()
);
#174=(
REPRESENTATION_RELATIONSHIP($,$,#15041,#15030)
REPRESENTATION_RELATIONSHIP_WITH_TRANSFORMATION(#91)
SHAPE_REPRESENTATION_RELATIONSHIP()
);
#175=(
REPRESENTATION_RELATIONSHIP($,$,#14999,#14998)
REPRESENTATION_RELATIONSHIP_WITH_TRANSFORMATION(#92)
SHAPE_REPRESENTATION_RELATIONSHIP()
);
#176=(
REPRESENTATION_RELATIONSHIP($,$,#15030,#14998)
REPRESENTATION_RELATIONSHIP_WITH_TRANSFORMATION(#93)
SHAPE_REPRESENTATION_RELATIONSHIP()
);
#177=CONTEXT_DEPENDENT_SHAPE_REPRESENTATION(#94,#14895);
#178=CONTEXT_DEPENDENT_SHAPE_REPRESENTATION(#95,#14896);
#179=CONTEXT_DEPENDENT_SHAPE_REPRESENTATION(#96,#14897);
#180=CONTEXT_DEPENDENT_SHAPE_REPRESENTATION(#97,#14898);
#181=CONTEXT_DEPENDENT_SHAPE_REPRESENTATION(#98,#14899);
#182=CONTEXT_DEPENDENT_SHAPE_REPRESENTATION(#99,#14906);
#183=CONTEXT_DEPENDENT_SHAPE_REPRESENTATION(#100,#14907);
#184=CONTEXT_DEPENDENT_SHAPE_REPRESENTATION(#101,#14908);
#185=CONTEXT_DEPENDENT_SHAPE_REPRESENTATION(#102,#14909);
#186=CONTEXT_DEPENDENT_SHAPE_REPRESENTATION(#103,#14910);
#187=CONTEXT_DEPENDENT_SHAPE_REPRESENTATION(#104,#14913);
#188=CONTEXT_DEPENDENT_SHAPE_REPRESENTATION(#105,#14914);
#189=CONTEXT_DEPENDENT_SHAPE_REPRESENTATION(#106,#14915);
#190=CONTEXT_DEPENDENT_SHAPE_REPRESENTATION(#107,#14916);
#191=CONTEXT_DEPENDENT_SHAPE_REPRESENTATION(#108,#14917);
#192=CONTEXT_DEPENDENT_SHAPE_REPRESENTATION(#109,#14918);
#193=CONTEXT_DEPENDENT_SHAPE_REPRESENTATION(#110,#14919);
#194=CONTEXT_DEPENDENT_SHAPE_REPRESENTATION(#111,#14920);
#195=CONTEXT_DEPENDENT_SHAPE_REPRESENTATION(#112,#14921);
#196=CONTEXT_DEPENDENT_SHAPE_REPRESENTATION(#113,#14922);
#197=CONTEXT_DEPENDENT_SHAPE_REPRESENTATION(#114,#14923);
#198=CONTEXT_DEPENDENT_SHAPE_REPRESENTATION(#115,#14924);
#199=CONTEXT_DEPENDENT_SHAPE_REPRESENTATION(#116,#14925);
#200=CONTEXT_DEPENDENT_SHAPE_REPRESENTATION(#117,#14926);
#201=CONTEXT_DEPENDENT_SHAPE_REPRESENTATION(#118,#14927);
#202=CONTEXT_DEPENDENT_SHAPE_REPRESENTATION(#119,#14928);
#203=CONTEXT_DEPENDENT_SHAPE_REPRESENTATION(#120,#14929);
#204=CONTEXT_DEPENDENT_SHAPE_REPRESENTATION(#121,#14930);
#205=CONTEXT_DEPENDENT_SHAPE_REPRESENTATION(#122,#14931);
#206=CONTEXT_DEPENDENT_SHAPE_REPRESENTATION(#123,#14932);
#207=CONTEXT_DEPENDENT_SHAPE_REPRESENTATION(#124,#14933);
#208=CONTEXT_DEPENDENT_SHAPE_REPRESENTATION(#125,#14934);
#209=CONTEXT_DEPENDENT_SHAPE_REPRESENTATION(#126,#14935);
#210=CONTEXT_DEPENDENT_SHAPE_REPRESENTATION(#127,#14936);
#211=CONTEXT_DEPENDENT_SHAPE_REPRESENTATION(#128,#14937);
#212=CONTEXT_DEPENDENT_SHAPE_REPRESENTATION(#129,#14938);
#213=CONTEXT_DEPENDENT_SHAPE_REPRESENTATION(#130,#14939);
#214=CONTEXT_DEPENDENT_SHAPE_REPRESENTATION(#131,#14940);
#215=CONTEXT_DEPENDENT_SHAPE_REPRESENTATION(#132,#14941);
#216=CONTEXT_DEPENDENT_SHAPE_REPRESENTATION(#133,#14942);
#217=CONTEXT_DEPENDENT_SHAPE_REPRESENTATION(#134,#14943);
#218=CONTEXT_DEPENDENT_SHAPE_REPRESENTATION(#135,#14944);
#219=CONTEXT_DEPENDENT_SHAPE_REPRESENTATION(#136,#14945);
#220=CONTEXT_DEPENDENT_SHAPE_REPRESENTATION(#137,#14946);
#221=CONTEXT_DEPENDENT_SHAPE_REPRESENTATION(#138,#14947);
#222=CONTEXT_DEPENDENT_SHAPE_REPRESENTATION(#139,#14948);
#223=CONTEXT_DEPENDENT_SHAPE_REPRESENTATION(#140,#14949);
#224=CONTEXT_DEPENDENT_SHAPE_REPRESENTATION(#141,#14950);
#225=CONTEXT_DEPENDENT_SHAPE_REPRESENTATION(#142,#14951);
#226=CONTEXT_DEPENDENT_SHAPE_REPRESENTATION(#143,#14952);
#227=CONTEXT_DEPENDENT_SHAPE_REPRESENTATION(#144,#14953);
#228=CONTEXT_DEPENDENT_SHAPE_REPRESENTATION(#145,#14954);
#229=CONTEXT_DEPENDENT_SHAPE_REPRESENTATION(#146,#14955);
#230=CONTEXT_DEPENDENT_SHAPE_REPRESENTATION(#147,#14956);
#231=CONTEXT_DEPENDENT_SHAPE_REPRESENTATION(#148,#14957);
#232=CONTEXT_DEPENDENT_SHAPE_REPRESENTATION(#149,#14958);
#233=CONTEXT_DEPENDENT_SHAPE_REPRESENTATION(#150,#14959);
#234=CONTEXT_DEPENDENT_SHAPE_REPRESENTATION(#151,#14960);
#235=CONTEXT_DEPENDENT_SHAPE_REPRESENTATION(#152,#14961);
#236=CONTEXT_DEPENDENT_SHAPE_REPRESENTATION(#153,#14962);
#237=CONTEXT_DEPENDENT_SHAPE_REPRESENTATION(#154,#14963);
#238=CONTEXT_DEPENDENT_SHAPE_REPRESENTATION(#155,#14964);
#239=CONTEXT_DEPENDENT_SHAPE_REPRESENTATION(#156,#14965);
#240=CONTEXT_DEPENDENT_SHAPE_REPRESENTATION(#157,#14966);
#241=CONTEXT_DEPENDENT_SHAPE_REPRESENTATION(#158,#14967);
#242=CONTEXT_DEPENDENT_SHAPE_REPRESENTATION(#159,#14968);
#243=CONTEXT_DEPENDENT_SHAPE_REPRESENTATION(#160,#14981);
#244=CONTEXT_DEPENDENT_SHAPE_REPRESENTATION(#161,#14982);
#245=CONTEXT_DEPENDENT_SHAPE_REPRESENTATION(#162,#14983);
#246=CONTEXT_DEPENDENT_SHAPE_REPRESENTATION(#163,#14984);
#247=CONTEXT_DEPENDENT_SHAPE_REPRESENTATION(#164,#14985);
#248=CONTEXT_DEPENDENT_SHAPE_REPRESENTATION(#165,#14986);
#249=CONTEXT_DEPENDENT_SHAPE_REPRESENTATION(#166,#14987);
#250=CONTEXT_DEPENDENT_SHAPE_REPRESENTATION(#167,#14988);
#251=CONTEXT_DEPENDENT_SHAPE_REPRESENTATION(#168,#14989);
#252=CONTEXT_DEPENDENT_SHAPE_REPRESENTATION(#169,#14990);
#253=CONTEXT_DEPENDENT_SHAPE_REPRESENTATION(#170,#14991);
#254=CONTEXT_DEPENDENT_SHAPE_REPRESENTATION(#171,#14992);
#255=CONTEXT_DEPENDENT_SHAPE_REPRESENTATION(#172,#14993);
#256=CONTEXT_DEPENDENT_SHAPE_REPRESENTATION(#173,#14994);
#257=CONTEXT_DEPENDENT_SHAPE_REPRESENTATION(#174,#14995);
#258=CONTEXT_DEPENDENT_SHAPE_REPRESENTATION(#175,#14996);
#259=CONTEXT_DEPENDENT_SHAPE_REPRESENTATION(#176,#14997);
#260=NEXT_ASSEMBLY_USAGE_OCCURRENCE('Inner ring:1','Inner ring:1',
'Inner ring:1',#15061,#15062,'Inner ring:1');
#261=NEXT_ASSEMBLY_USAGE_OCCURRENCE('Outer ring:1','Outer ring:1',
'Outer ring:1',#15061,#15063,'Outer ring:1');
#262=NEXT_ASSEMBLY_USAGE_OCCURRENCE('Balls:1','Balls:1','Balls:1',#15061,
#15064,'Balls:1');
#263=NEXT_ASSEMBLY_USAGE_OCCURRENCE('Cage:1','Cage:1','Cage:1',#15061,#15065,
'Cage:1');
#264=NEXT_ASSEMBLY_USAGE_OCCURRENCE('Seals 2RS:1','Seals 2RS:1',
'Seals 2RS:1',#15061,#15066,'Seals 2RS:1');
#265=NEXT_ASSEMBLY_USAGE_OCCURRENCE('Inner ring (1):1',
'Inner ring (1):1','Inner ring (1):1',#15067,#15068,'Inner ring (1):1');
#266=NEXT_ASSEMBLY_USAGE_OCCURRENCE('Outer ring (1):1',
'Outer ring (1):1','Outer ring (1):1',#15067,#15069,'Outer ring (1):1');
#267=NEXT_ASSEMBLY_USAGE_OCCURRENCE('Balls (1):1','Balls (1):1',
'Balls (1):1',#15067,#15070,'Balls (1):1');
#268=NEXT_ASSEMBLY_USAGE_OCCURRENCE('Cage (1):1','Cage (1):1',
'Cage (1):1',#15067,#15071,'Cage (1):1');
#269=NEXT_ASSEMBLY_USAGE_OCCURRENCE('Seals 2RS (1):1','Seals 2RS (1):1',
'Seals 2RS (1):1',#15067,#15072,'Seals 2RS (1):1');
#270=NEXT_ASSEMBLY_USAGE_OCCURRENCE('Base:1','Base:1','Base:1',#15044,#15045,
'Base:1');
#271=NEXT_ASSEMBLY_USAGE_OCCURRENCE('Support housing:1',
'Support housing:1','Support housing:1',#15044,#15046,
'Support housing:1');
#272=NEXT_ASSEMBLY_USAGE_OCCURRENCE('Support cap:1','Support cap:1',
'Support cap:1',#15044,#15047,'Support cap:1');
#273=NEXT_ASSEMBLY_USAGE_OCCURRENCE('Support cap (1):1',
'Support cap (1):1','Support cap (1):1',#15044,#15048,
'Support cap (1):1');
#274=NEXT_ASSEMBLY_USAGE_OCCURRENCE('Support housing (1):1',
'Support housing (1):1','Support housing (1):1',#15044,#15049,
'Support housing (1):1');
#275=NEXT_ASSEMBLY_USAGE_OCCURRENCE('Support cap (2):1',
'Support cap (2):1','Support cap (2):1',#15044,#15050,
'Support cap (2):1');
#276=NEXT_ASSEMBLY_USAGE_OCCURRENCE('Support cap (3):1',
'Support cap (3):1','Support cap (3):1',#15044,#15051,
'Support cap (3):1');
#277=NEXT_ASSEMBLY_USAGE_OCCURRENCE('Reaction housing and arm:1',
'Reaction housing and arm:1','Reaction housing and arm:1',#15044,#15052,
'Reaction housing and arm:1');
#278=NEXT_ASSEMBLY_USAGE_OCCURRENCE('Test bearing cap:1',
'Test bearing cap:1','Test bearing cap:1',#15044,#15053,
'Test bearing cap:1');
#279=NEXT_ASSEMBLY_USAGE_OCCURRENCE('Test bearing cap (1):1',
'Test bearing cap (1):1','Test bearing cap (1):1',#15044,#15054,
'Test bearing cap (1):1');
#280=NEXT_ASSEMBLY_USAGE_OCCURRENCE('Sensor pedestal:1',
'Sensor pedestal:1','Sensor pedestal:1',#15044,#15055,
'Sensor pedestal:1');
#281=NEXT_ASSEMBLY_USAGE_OCCURRENCE('Load cell envelope:1',
'Load cell envelope:1','Load cell envelope:1',#15044,#15056,
'Load cell envelope:1');
#282=NEXT_ASSEMBLY_USAGE_OCCURRENCE('Protective frame:1',
'Protective frame:1','Protective frame:1',#15044,#15057,
'Protective frame:1');
#283=NEXT_ASSEMBLY_USAGE_OCCURRENCE('Foot pad:1','Foot pad:1',
'Foot pad:1',#15044,#15058,'Foot pad:1');
#284=NEXT_ASSEMBLY_USAGE_OCCURRENCE('Foot pad (1):1','Foot pad (1):1',
'Foot pad (1):1',#15044,#15059,'Foot pad (1):1');
#285=NEXT_ASSEMBLY_USAGE_OCCURRENCE('M6x18 mounting screw:2',
'M6x18 mounting screw:2','M6x18 mounting screw:2',#15044,#15060,
'M6x18 mounting screw:2');
#286=NEXT_ASSEMBLY_USAGE_OCCURRENCE('M6x18 mounting screw:3',
'M6x18 mounting screw:3','M6x18 mounting screw:3',#15044,#15060,
'M6x18 mounting screw:3');
#287=NEXT_ASSEMBLY_USAGE_OCCURRENCE(
'Sealed Ball Bearing - 12 x 32 x 10 mm:2',
'Sealed Ball Bearing - 12 x 32 x 10 mm:2',
'Sealed Ball Bearing - 12 x 32 x 10 mm:2',#15044,#15061,
'Sealed Ball Bearing - 12 x 32 x 10 mm:2');
#288=NEXT_ASSEMBLY_USAGE_OCCURRENCE('M4x10 Cap Screw:2',
'M4x10 Cap Screw:2','M4x10 Cap Screw:2',#15044,#15074,
'M4x10 Cap Screw:2');
#289=NEXT_ASSEMBLY_USAGE_OCCURRENCE('M4x10 Cap Screw:3',
'M4x10 Cap Screw:3','M4x10 Cap Screw:3',#15044,#15074,
'M4x10 Cap Screw:3');
#290=NEXT_ASSEMBLY_USAGE_OCCURRENCE('M4x10 Cap Screw:4',
'M4x10 Cap Screw:4','M4x10 Cap Screw:4',#15044,#15074,
'M4x10 Cap Screw:4');
#291=NEXT_ASSEMBLY_USAGE_OCCURRENCE('M4x10 Cap Screw:5',
'M4x10 Cap Screw:5','M4x10 Cap Screw:5',#15044,#15074,
'M4x10 Cap Screw:5');
#292=NEXT_ASSEMBLY_USAGE_OCCURRENCE('M4x10 Cap Screw:6',
'M4x10 Cap Screw:6','M4x10 Cap Screw:6',#15044,#15074,
'M4x10 Cap Screw:6');
#293=NEXT_ASSEMBLY_USAGE_OCCURRENCE('M4x10 Cap Screw:7',
'M4x10 Cap Screw:7','M4x10 Cap Screw:7',#15044,#15074,
'M4x10 Cap Screw:7');
#294=NEXT_ASSEMBLY_USAGE_OCCURRENCE('M4x10 Cap Screw:8',
'M4x10 Cap Screw:8','M4x10 Cap Screw:8',#15044,#15074,
'M4x10 Cap Screw:8');
#295=NEXT_ASSEMBLY_USAGE_OCCURRENCE('M4x10 Cap Screw:9',
'M4x10 Cap Screw:9','M4x10 Cap Screw:9',#15044,#15074,
'M4x10 Cap Screw:9');
#296=NEXT_ASSEMBLY_USAGE_OCCURRENCE('M6x18 mounting screw:4',
'M6x18 mounting screw:4','M6x18 mounting screw:4',#15044,#15060,
'M6x18 mounting screw:4');
#297=NEXT_ASSEMBLY_USAGE_OCCURRENCE('M6x18 mounting screw:5',
'M6x18 mounting screw:5','M6x18 mounting screw:5',#15044,#15060,
'M6x18 mounting screw:5');
#298=NEXT_ASSEMBLY_USAGE_OCCURRENCE(
'Sealed Ball Bearing - 12 x 32 x 10 mm:3',
'Sealed Ball Bearing - 12 x 32 x 10 mm:3',
'Sealed Ball Bearing - 12 x 32 x 10 mm:3',#15044,#15061,
'Sealed Ball Bearing - 12 x 32 x 10 mm:3');
#299=NEXT_ASSEMBLY_USAGE_OCCURRENCE('M4x10 Cap Screw:10',
'M4x10 Cap Screw:10','M4x10 Cap Screw:10',#15044,#15074,
'M4x10 Cap Screw:10');
#300=NEXT_ASSEMBLY_USAGE_OCCURRENCE('M4x10 Cap Screw:11',
'M4x10 Cap Screw:11','M4x10 Cap Screw:11',#15044,#15074,
'M4x10 Cap Screw:11');
#301=NEXT_ASSEMBLY_USAGE_OCCURRENCE('M4x10 Cap Screw:12',
'M4x10 Cap Screw:12','M4x10 Cap Screw:12',#15044,#15074,
'M4x10 Cap Screw:12');
#302=NEXT_ASSEMBLY_USAGE_OCCURRENCE('M4x10 Cap Screw:13',
'M4x10 Cap Screw:13','M4x10 Cap Screw:13',#15044,#15074,
'M4x10 Cap Screw:13');
#303=NEXT_ASSEMBLY_USAGE_OCCURRENCE('M4x10 Cap Screw:14',
'M4x10 Cap Screw:14','M4x10 Cap Screw:14',#15044,#15074,
'M4x10 Cap Screw:14');
#304=NEXT_ASSEMBLY_USAGE_OCCURRENCE('M4x10 Cap Screw:15',
'M4x10 Cap Screw:15','M4x10 Cap Screw:15',#15044,#15074,
'M4x10 Cap Screw:15');
#305=NEXT_ASSEMBLY_USAGE_OCCURRENCE('M4x10 Cap Screw:16',
'M4x10 Cap Screw:16','M4x10 Cap Screw:16',#15044,#15074,
'M4x10 Cap Screw:16');
#306=NEXT_ASSEMBLY_USAGE_OCCURRENCE('M4x10 Cap Screw:17',
'M4x10 Cap Screw:17','M4x10 Cap Screw:17',#15044,#15074,
'M4x10 Cap Screw:17');
#307=NEXT_ASSEMBLY_USAGE_OCCURRENCE(
'Sealed Ball Bearing - 20 x 47 x 14 mm:2',
'Sealed Ball Bearing - 20 x 47 x 14 mm:2',
'Sealed Ball Bearing - 20 x 47 x 14 mm:2',#15044,#15067,
'Sealed Ball Bearing - 20 x 47 x 14 mm:2');
#308=NEXT_ASSEMBLY_USAGE_OCCURRENCE('M4x10 Cap Screw:18',
'M4x10 Cap Screw:18','M4x10 Cap Screw:18',#15044,#15074,
'M4x10 Cap Screw:18');
#309=NEXT_ASSEMBLY_USAGE_OCCURRENCE('M4x10 Cap Screw:19',
'M4x10 Cap Screw:19','M4x10 Cap Screw:19',#15044,#15074,
'M4x10 Cap Screw:19');
#310=NEXT_ASSEMBLY_USAGE_OCCURRENCE('M4x10 Cap Screw:20',
'M4x10 Cap Screw:20','M4x10 Cap Screw:20',#15044,#15074,
'M4x10 Cap Screw:20');
#311=NEXT_ASSEMBLY_USAGE_OCCURRENCE('M4x10 Cap Screw:21',
'M4x10 Cap Screw:21','M4x10 Cap Screw:21',#15044,#15074,
'M4x10 Cap Screw:21');
#312=NEXT_ASSEMBLY_USAGE_OCCURRENCE('M4x10 Cap Screw:22',
'M4x10 Cap Screw:22','M4x10 Cap Screw:22',#15044,#15074,
'M4x10 Cap Screw:22');
#313=NEXT_ASSEMBLY_USAGE_OCCURRENCE('M4x10 Cap Screw:23',
'M4x10 Cap Screw:23','M4x10 Cap Screw:23',#15044,#15074,
'M4x10 Cap Screw:23');
#314=NEXT_ASSEMBLY_USAGE_OCCURRENCE('M4x10 Cap Screw:24',
'M4x10 Cap Screw:24','M4x10 Cap Screw:24',#15044,#15074,
'M4x10 Cap Screw:24');
#315=NEXT_ASSEMBLY_USAGE_OCCURRENCE('M4x10 Cap Screw:25',
'M4x10 Cap Screw:25','M4x10 Cap Screw:25',#15044,#15074,
'M4x10 Cap Screw:25');
#316=NEXT_ASSEMBLY_USAGE_OCCURRENCE('Cap Screw - M5x20:2',
'Cap Screw - M5x20:2','Cap Screw - M5x20:2',#15044,#15073,
'Cap Screw - M5x20:2');
#317=NEXT_ASSEMBLY_USAGE_OCCURRENCE('Cap Screw - M5x20:3',
'Cap Screw - M5x20:3','Cap Screw - M5x20:3',#15044,#15073,
'Cap Screw - M5x20:3');
#318=NEXT_ASSEMBLY_USAGE_OCCURRENCE('Cap Screw - M5x20:4',
'Cap Screw - M5x20:4','Cap Screw - M5x20:4',#15044,#15073,
'Cap Screw - M5x20:4');
#319=NEXT_ASSEMBLY_USAGE_OCCURRENCE('Cap Screw - M5x20:5',
'Cap Screw - M5x20:5','Cap Screw - M5x20:5',#15044,#15073,
'Cap Screw - M5x20:5');
#320=NEXT_ASSEMBLY_USAGE_OCCURRENCE('M4x10 Cap Screw:26',
'M4x10 Cap Screw:26','M4x10 Cap Screw:26',#15044,#15074,
'M4x10 Cap Screw:26');
#321=NEXT_ASSEMBLY_USAGE_OCCURRENCE('M4x10 Cap Screw:27',
'M4x10 Cap Screw:27','M4x10 Cap Screw:27',#15044,#15074,
'M4x10 Cap Screw:27');
#322=NEXT_ASSEMBLY_USAGE_OCCURRENCE('M4x10 Cap Screw:28',
'M4x10 Cap Screw:28','M4x10 Cap Screw:28',#15044,#15074,
'M4x10 Cap Screw:28');
#323=NEXT_ASSEMBLY_USAGE_OCCURRENCE('M4x10 Cap Screw:29',
'M4x10 Cap Screw:29','M4x10 Cap Screw:29',#15044,#15074,
'M4x10 Cap Screw:29');
#324=NEXT_ASSEMBLY_USAGE_OCCURRENCE('M4x10 Cap Screw:30',
'M4x10 Cap Screw:30','M4x10 Cap Screw:30',#15044,#15074,
'M4x10 Cap Screw:30');
#325=NEXT_ASSEMBLY_USAGE_OCCURRENCE('M4x10 Cap Screw:31',
'M4x10 Cap Screw:31','M4x10 Cap Screw:31',#15044,#15074,
'M4x10 Cap Screw:31');
#326=NEXT_ASSEMBLY_USAGE_OCCURRENCE('Stepped arbor:1','Stepped arbor:1',
'Stepped arbor:1',#15075,#15076,'Stepped arbor:1');
#327=NEXT_ASSEMBLY_USAGE_OCCURRENCE('Support inner spacer:1',
'Support inner spacer:1','Support inner spacer:1',#15075,#15077,
'Support inner spacer:1');
#328=NEXT_ASSEMBLY_USAGE_OCCURRENCE('Support inner spacer (1):1',
'Support inner spacer (1):1','Support inner spacer (1):1',#15075,#15078,
'Support inner spacer (1):1');
#329=NEXT_ASSEMBLY_USAGE_OCCURRENCE('Journal collar:1',
'Journal collar:1','Journal collar:1',#15075,#15079,'Journal collar:1');
#330=NEXT_ASSEMBLY_USAGE_OCCURRENCE('Journal collar (1):1',
'Journal collar (1):1','Journal collar (1):1',#15075,#15080,
'Journal collar (1):1');
#331=NEXT_ASSEMBLY_USAGE_OCCURRENCE('Outer journal spacer:1',
'Outer journal spacer:1','Outer journal spacer:1',#15075,#15081,
'Outer journal spacer:1');
#332=NEXT_ASSEMBLY_USAGE_OCCURRENCE('Outer journal spacer (1):1',
'Outer journal spacer (1):1','Outer journal spacer (1):1',#15075,#15082,
'Outer journal spacer (1):1');
#333=NEXT_ASSEMBLY_USAGE_OCCURRENCE('Test bearing collar:1',
'Test bearing collar:1','Test bearing collar:1',#15075,#15083,
'Test bearing collar:1');
#334=NEXT_ASSEMBLY_USAGE_OCCURRENCE('Test bearing collar (1):1',
'Test bearing collar (1):1','Test bearing collar (1):1',#15075,#15084,
'Test bearing collar (1):1');
#335=NEXT_ASSEMBLY_USAGE_OCCURRENCE('Drive flange:1','Drive flange:1',
'Drive flange:1',#15075,#15085,'Drive flange:1');
#336=NEXT_ASSEMBLY_USAGE_OCCURRENCE('Socket Set Screw - M5x8:2',
'Socket Set Screw - M5x8:2','Socket Set Screw - M5x8:2',#15075,#15086,
'Socket Set Screw - M5x8:2');
#337=NEXT_ASSEMBLY_USAGE_OCCURRENCE('Socket Set Screw - M5x8:3',
'Socket Set Screw - M5x8:3','Socket Set Screw - M5x8:3',#15075,#15086,
'Socket Set Screw - M5x8:3');
#338=NEXT_ASSEMBLY_USAGE_OCCURRENCE('Socket Set Screw - M5x8:4',
'Socket Set Screw - M5x8:4','Socket Set Screw - M5x8:4',#15075,#15086,
'Socket Set Screw - M5x8:4');
#339=NEXT_ASSEMBLY_USAGE_OCCURRENCE('Socket Set Screw - M5x8:5',
'Socket Set Screw - M5x8:5','Socket Set Screw - M5x8:5',#15075,#15086,
'Socket Set Screw - M5x8:5');
#340=NEXT_ASSEMBLY_USAGE_OCCURRENCE('Socket Set Screw - M5x8:6',
'Socket Set Screw - M5x8:6','Socket Set Screw - M5x8:6',#15075,#15086,
'Socket Set Screw - M5x8:6');
#341=NEXT_ASSEMBLY_USAGE_OCCURRENCE('Supports and reaction sensor:1',
'Supports and reaction sensor:1','Supports and reaction sensor:1',#15043,
#15044,'Supports and reaction sensor:1');
#342=NEXT_ASSEMBLY_USAGE_OCCURRENCE('Test arbor and drive flange:1',
'Test arbor and drive flange:1','Test arbor and drive flange:1',#15043,
#15075,'Test arbor and drive flange:1');
#343=B_SPLINE_CURVE_WITH_KNOTS('',3,(#12896,#12897,#12898,#12899,#12900,
#12901,#12902,#12903,#12904,#12905,#12906,#12907,#12908,#12909,#12910,#12911,
#12912,#12913,#12914,#12915,#12916,#12917),.UNSPECIFIED.,.F.,.F.,(4,2,2,
2,2,2,2,2,2,2,4),(0.0591825211272536,0.157966726598481,0.236950089897721,
0.315933453196962,0.391576304923761,0.46721915665056,0.54286200837736,0.618504860104159,
0.697488223403399,0.77647158670264,0.875255792173867),.UNSPECIFIED.);
#344=B_SPLINE_CURVE_WITH_KNOTS('',3,(#12921,#12922,#12923,#12924,#12925,
#12926,#12927,#12928,#12929,#12930,#12931,#12932,#12933,#12934,#12935,#12936,
#12937,#12938,#12939,#12940,#12941,#12942),.UNSPECIFIED.,.F.,.F.,(4,2,2,
2,2,2,2,2,2,2,4),(0.0581119756758434,0.106553146291161,0.213106292582322,
0.30849933801665,0.386091982889075,0.4636846277615,0.541277272633925,0.61886991750635,
0.714262962940678,0.820816109231839,0.869257279847157),.UNSPECIFIED.);
#345=B_SPLINE_CURVE_WITH_KNOTS('',3,(#12948,#12949,#12950,#12951,#12952,
#12953,#12954,#12955,#12956,#12957,#12958,#12959,#12960,#12961,#12962,#12963,
#12964,#12965,#12966,#12967,#12968,#12969),.UNSPECIFIED.,.F.,.F.,(4,2,2,
2,2,2,2,2,2,2,4),(0.0581119756758434,0.106553146291161,0.213106292582322,
0.30849933801665,0.386091982889075,0.4636846277615,0.541277272633925,0.61886991750635,
0.714262962940679,0.820816109231839,0.869257279847157),.UNSPECIFIED.);
#346=B_SPLINE_CURVE_WITH_KNOTS('',3,(#12973,#12974,#12975,#12976,#12977,
#12978,#12979,#12980,#12981,#12982,#12983,#12984,#12985,#12986,#12987,#12988,
#12989,#12990,#12991,#12992,#12993,#12994),.UNSPECIFIED.,.F.,.F.,(4,2,2,
2,2,2,2,2,2,2,4),(0.0581119756758433,0.106553146291161,0.213106292582322,
0.308499338016649,0.386091982889075,0.4636846277615,0.541277272633925,0.61886991750635,
0.714262962940678,0.820816109231839,0.869257279847157),.UNSPECIFIED.);
#347=B_SPLINE_CURVE_WITH_KNOTS('',3,(#13003,#13004,#13005,#13006,#13007,
#13008,#13009,#13010,#13011,#13012,#13013,#13014,#13015,#13016,#13017,#13018,
#13019,#13020,#13021,#13022,#13023,#13024),.UNSPECIFIED.,.F.,.F.,(4,2,2,
2,2,2,2,2,2,2,4),(0.0581119756758433,0.106553146291161,0.213106292582322,
0.30849933801665,0.386091982889075,0.4636846277615,0.541277272633925,0.61886991750635,
0.714262962940678,0.820816109231839,0.869257279847157),.UNSPECIFIED.);
#348=B_SPLINE_CURVE_WITH_KNOTS('',3,(#13028,#13029,#13030,#13031,#13032,
#13033,#13034,#13035,#13036,#13037,#13038,#13039,#13040,#13041,#13042,#13043,
#13044,#13045,#13046,#13047,#13048,#13049),.UNSPECIFIED.,.F.,.F.,(4,2,2,
2,2,2,2,2,2,2,4),(0.0581119756758434,0.106553146291161,0.213106292582322,
0.30849933801665,0.386091982889075,0.4636846277615,0.541277272633925,0.61886991750635,
0.714262962940678,0.820816109231839,0.869257279847157),.UNSPECIFIED.);
#349=B_SPLINE_CURVE_WITH_KNOTS('',3,(#13053,#13054,#13055,#13056,#13057,
#13058,#13059,#13060,#13061,#13062,#13063,#13064,#13065,#13066,#13067,#13068,
#13069,#13070,#13071,#13072,#13073,#13074),.UNSPECIFIED.,.F.,.F.,(4,2,2,
2,2,2,2,2,2,2,4),(0.0581119756758434,0.106553146291161,0.213106292582322,
0.30849933801665,0.386091982889075,0.4636846277615,0.541277272633925,0.61886991750635,
0.714262962940678,0.820816109231839,0.869257279847157),.UNSPECIFIED.);
#350=B_SPLINE_CURVE_WITH_KNOTS('',3,(#13078,#13079,#13080,#13081,#13082,
#13083,#13084,#13085,#13086,#13087,#13088,#13089,#13090,#13091,#13092,#13093,
#13094,#13095,#13096,#13097,#13098,#13099),.UNSPECIFIED.,.F.,.F.,(4,2,2,
2,2,2,2,2,2,2,4),(0.0581119756758433,0.106553146291161,0.213106292582322,
0.30849933801665,0.386091982889075,0.4636846277615,0.541277272633925,0.61886991750635,
0.714262962940678,0.820816109231839,0.869257279847157),.UNSPECIFIED.);
#351=B_SPLINE_CURVE_WITH_KNOTS('',3,(#13107,#13108,#13109,#13110,#13111,
#13112,#13113,#13114,#13115,#13116,#13117,#13118,#13119,#13120,#13121,#13122,
#13123,#13124,#13125,#13126,#13127,#13128),.UNSPECIFIED.,.F.,.F.,(4,2,2,
2,2,2,2,2,2,2,4),(0.0591825211272536,0.157966726598481,0.236950089897721,
0.315933453196962,0.391576304923761,0.467219156650561,0.54286200837736,
0.618504860104159,0.697488223403399,0.77647158670264,0.875255792173867),
 .UNSPECIFIED.);
#352=B_SPLINE_CURVE_WITH_KNOTS('',3,(#13136,#13137,#13138,#13139,#13140,
#13141,#13142,#13143,#13144,#13145,#13146,#13147,#13148,#13149,#13150,#13151,
#13152,#13153,#13154,#13155,#13156,#13157),.UNSPECIFIED.,.F.,.F.,(4,2,2,
2,2,2,2,2,2,2,4),(0.0591825211272536,0.157966726598481,0.236950089897722,
0.315933453196962,0.391576304923761,0.467219156650561,0.54286200837736,
0.618504860104159,0.697488223403399,0.77647158670264,0.875255792173867),
 .UNSPECIFIED.);
#353=B_SPLINE_CURVE_WITH_KNOTS('',3,(#13167,#13168,#13169,#13170,#13171,
#13172,#13173,#13174,#13175,#13176,#13177,#13178,#13179,#13180,#13181,#13182,
#13183,#13184,#13185,#13186,#13187,#13188),.UNSPECIFIED.,.F.,.F.,(4,2,2,
2,2,2,2,2,2,2,4),(0.0591825211272536,0.157966726598481,0.236950089897721,
0.315933453196962,0.391576304923761,0.46721915665056,0.54286200837736,0.618504860104159,
0.697488223403399,0.77647158670264,0.875255792173867),.UNSPECIFIED.);
#354=B_SPLINE_CURVE_WITH_KNOTS('',3,(#13196,#13197,#13198,#13199,#13200,
#13201,#13202,#13203,#13204,#13205,#13206,#13207,#13208,#13209,#13210,#13211,
#13212,#13213,#13214,#13215,#13216,#13217),.UNSPECIFIED.,.F.,.F.,(4,2,2,
2,2,2,2,2,2,2,4),(0.0591825211272536,0.157966726598481,0.236950089897721,
0.315933453196962,0.391576304923761,0.46721915665056,0.542862008377359,
0.618504860104159,0.697488223403399,0.776471586702639,0.875255792173867),
 .UNSPECIFIED.);
#355=B_SPLINE_CURVE_WITH_KNOTS('',3,(#13225,#13226,#13227,#13228,#13229,
#13230,#13231,#13232,#13233,#13234,#13235,#13236,#13237,#13238,#13239,#13240,
#13241,#13242,#13243,#13244,#13245,#13246),.UNSPECIFIED.,.F.,.F.,(4,2,2,
2,2,2,2,2,2,2,4),(0.0591825211272536,0.157966726598481,0.236950089897721,
0.315933453196962,0.391576304923761,0.46721915665056,0.54286200837736,0.618504860104159,
0.697488223403399,0.77647158670264,0.875255792173867),.UNSPECIFIED.);
#356=B_SPLINE_CURVE_WITH_KNOTS('',3,(#13255,#13256,#13257,#13258,#13259,
#13260,#13261,#13262,#13263,#13264,#13265,#13266,#13267,#13268,#13269,#13270,
#13271,#13272,#13273,#13274,#13275,#13276),.UNSPECIFIED.,.F.,.F.,(4,2,2,
2,2,2,2,2,2,2,4),(0.0591825211272536,0.157966726598481,0.236950089897721,
0.315933453196962,0.391576304923761,0.46721915665056,0.542862008377359,
0.618504860104159,0.697488223403399,0.776471586702639,0.875255792173867),
 .UNSPECIFIED.);
#357=B_SPLINE_CURVE_WITH_KNOTS('',3,(#13426,#13427,#13428,#13429,#13430,
#13431,#13432,#13433,#13434,#13435,#13436,#13437,#13438,#13439,#13440,#13441,
#13442,#13443,#13444,#13445,#13446,#13447),.UNSPECIFIED.,.F.,.F.,(4,2,2,
2,2,2,2,2,2,2,4),(0.0789094028588958,0.210573405340968,0.315860108011452,
0.421146810681936,0.522142632548711,0.623138454415485,0.72413427628226,
0.825130098149035,0.930416800819519,1.03570350349,1.16736750597208),
 .UNSPECIFIED.);
#358=B_SPLINE_CURVE_WITH_KNOTS('',3,(#13451,#13452,#13453,#13454,#13455,
#13456,#13457,#13458,#13459,#13460,#13461,#13462,#13463,#13464,#13465,#13466,
#13467,#13468,#13469,#13470,#13471,#13472),.UNSPECIFIED.,.F.,.F.,(4,2,2,
2,2,2,2,2,2,2,4),(0.0774793363974613,0.142088896491891,0.284177792983782,
0.411119756996526,0.514392970548519,0.617666184100513,0.720939397652506,
0.8242126112045,0.951154575217244,1.09324347170913,1.15785303180356),
 .UNSPECIFIED.);
#359=B_SPLINE_CURVE_WITH_KNOTS('',3,(#13478,#13479,#13480,#13481,#13482,
#13483,#13484,#13485,#13486,#13487,#13488,#13489,#13490,#13491,#13492,#13493,
#13494,#13495,#13496,#13497,#13498,#13499),.UNSPECIFIED.,.F.,.F.,(4,2,2,
2,2,2,2,2,2,2,4),(0.0774793363974613,0.142088896491891,0.284177792983782,
0.411119756996525,0.514392970548519,0.617666184100513,0.720939397652506,
0.8242126112045,0.951154575217243,1.09324347170913,1.15785303180356),
 .UNSPECIFIED.);
#360=B_SPLINE_CURVE_WITH_KNOTS('',3,(#13503,#13504,#13505,#13506,#13507,
#13508,#13509,#13510,#13511,#13512,#13513,#13514,#13515,#13516,#13517,#13518,
#13519,#13520,#13521,#13522,#13523,#13524),.UNSPECIFIED.,.F.,.F.,(4,2,2,
2,2,2,2,2,2,2,4),(0.0774793363974614,0.142088896491891,0.284177792983781,
0.411119756996525,0.514392970548519,0.617666184100512,0.720939397652506,
0.824212611204499,0.951154575217243,1.09324347170913,1.15785303180356),
 .UNSPECIFIED.);
#361=B_SPLINE_CURVE_WITH_KNOTS('',3,(#13528,#13529,#13530,#13531,#13532,
#13533,#13534,#13535,#13536,#13537,#13538,#13539),.UNSPECIFIED.,.F.,.F.,
(4,2,2,2,2,4),(0.0774793363974613,0.142088896491891,0.284177792983781,0.411119756996525,
0.514392970548519,0.617666184100512),.UNSPECIFIED.);
#362=B_SPLINE_CURVE_WITH_KNOTS('',3,(#13544,#13545,#13546,#13547,#13548,
#13549,#13550,#13551,#13552,#13553,#13554,#13555),.UNSPECIFIED.,.F.,.F.,
(4,2,2,2,2,4),(0.617666184100512,0.720939397652506,0.824212611204499,0.951154575217243,
1.09324347170913,1.15785303180356),.UNSPECIFIED.);
#363=B_SPLINE_CURVE_WITH_KNOTS('',3,(#13559,#13560,#13561,#13562,#13563,
#13564,#13565,#13566,#13567,#13568,#13569,#13570,#13571,#13572,#13573,#13574,
#13575,#13576,#13577,#13578,#13579,#13580),.UNSPECIFIED.,.F.,.F.,(4,2,2,
2,2,2,2,2,2,2,4),(0.0774793363974613,0.142088896491891,0.284177792983782,
0.411119756996526,0.514392970548519,0.617666184100513,0.720939397652507,
0.8242126112045,0.951154575217245,1.09324347170914,1.15785303180356),
 .UNSPECIFIED.);
#364=B_SPLINE_CURVE_WITH_KNOTS('',3,(#13584,#13585,#13586,#13587,#13588,
#13589,#13590,#13591,#13592,#13593,#13594,#13595,#13596,#13597,#13598,#13599,
#13600,#13601,#13602,#13603,#13604,#13605),.UNSPECIFIED.,.F.,.F.,(4,2,2,
2,2,2,2,2,2,2,4),(0.0774793363974613,0.142088896491891,0.284177792983782,
0.411119756996526,0.514392970548519,0.617666184100513,0.720939397652506,
0.824212611204499,0.951154575217243,1.09324347170913,1.15785303180356),
 .UNSPECIFIED.);
#365=B_SPLINE_CURVE_WITH_KNOTS('',3,(#13609,#13610,#13611,#13612,#13613,
#13614,#13615,#13616,#13617,#13618,#13619,#13620,#13621,#13622,#13623,#13624,
#13625,#13626,#13627,#13628,#13629,#13630),.UNSPECIFIED.,.F.,.F.,(4,2,2,
2,2,2,2,2,2,2,4),(0.0774793363974613,0.142088896491891,0.284177792983782,
0.411119756996526,0.514392970548519,0.617666184100513,0.720939397652506,
0.8242126112045,0.951154575217244,1.09324347170913,1.15785303180356),
 .UNSPECIFIED.);
#366=B_SPLINE_CURVE_WITH_KNOTS('',3,(#13634,#13635,#13636,#13637,#13638,
#13639,#13640,#13641,#13642,#13643,#13644,#13645,#13646,#13647,#13648,#13649,
#13650,#13651,#13652,#13653,#13654,#13655),.UNSPECIFIED.,.F.,.F.,(4,2,2,
2,2,2,2,2,2,2,4),(0.0774793363974613,0.142088896491891,0.284177792983782,
0.411119756996526,0.514392970548519,0.617666184100513,0.720939397652506,
0.8242126112045,0.951154575217243,1.09324347170913,1.15785303180356),
 .UNSPECIFIED.);
#367=B_SPLINE_CURVE_WITH_KNOTS('',3,(#13663,#13664,#13665,#13666,#13667,
#13668,#13669,#13670,#13671,#13672,#13673,#13674,#13675,#13676,#13677,#13678,
#13679,#13680,#13681,#13682,#13683,#13684),.UNSPECIFIED.,.F.,.F.,(4,2,2,
2,2,2,2,2,2,2,4),(0.0789094028588958,0.210573405340968,0.315860108011452,
0.421146810681936,0.522142632548711,0.623138454415485,0.72413427628226,
0.825130098149035,0.930416800819519,1.03570350349,1.16736750597208),
 .UNSPECIFIED.);
#368=B_SPLINE_CURVE_WITH_KNOTS('',3,(#13692,#13693,#13694,#13695,#13696,
#13697,#13698,#13699,#13700,#13701,#13702,#13703,#13704,#13705,#13706,#13707,
#13708,#13709,#13710,#13711,#13712,#13713),.UNSPECIFIED.,.F.,.F.,(4,2,2,
2,2,2,2,2,2,2,4),(0.0789094028588958,0.210573405340969,0.315860108011453,
0.421146810681937,0.522142632548712,0.623138454415486,0.724134276282261,
0.825130098149035,0.930416800819519,1.03570350349,1.16736750597208),
 .UNSPECIFIED.);
#369=B_SPLINE_CURVE_WITH_KNOTS('',3,(#13722,#13723,#13724,#13725,#13726,
#13727,#13728,#13729,#13730,#13731,#13732,#13733),.UNSPECIFIED.,.F.,.F.,
(4,2,2,2,2,4),(0.0789094028588958,0.210573405340968,0.315860108011452,0.421146810681937,
0.522142632548711,0.623138454415486),.UNSPECIFIED.);
#370=B_SPLINE_CURVE_WITH_KNOTS('',3,(#13735,#13736,#13737,#13738,#13739,
#13740,#13741,#13742,#13743,#13744,#13745,#13746),.UNSPECIFIED.,.F.,.F.,
(4,2,2,2,2,4),(0.623138454415486,0.72413427628226,0.825130098149035,0.930416800819519,
1.03570350349,1.16736750597208),.UNSPECIFIED.);
#371=B_SPLINE_CURVE_WITH_KNOTS('',3,(#13753,#13754,#13755,#13756,#13757,
#13758,#13759,#13760,#13761,#13762,#13763,#13764,#13765,#13766,#13767,#13768,
#13769,#13770,#13771,#13772,#13773,#13774),.UNSPECIFIED.,.F.,.F.,(4,2,2,
2,2,2,2,2,2,2,4),(0.0789094028588958,0.210573405340968,0.315860108011452,
0.421146810681936,0.522142632548711,0.623138454415486,0.72413427628226,
0.825130098149035,0.930416800819519,1.03570350349,1.16736750597208),
 .UNSPECIFIED.);
#372=B_SPLINE_CURVE_WITH_KNOTS('',3,(#13782,#13783,#13784,#13785,#13786,
#13787,#13788,#13789,#13790,#13791,#13792,#13793,#13794,#13795,#13796,#13797,
#13798,#13799,#13800,#13801,#13802,#13803),.UNSPECIFIED.,.F.,.F.,(4,2,2,
2,2,2,2,2,2,2,4),(0.0789094028588957,0.210573405340968,0.315860108011452,
0.421146810681936,0.522142632548711,0.623138454415485,0.72413427628226,
0.825130098149035,0.930416800819519,1.03570350349,1.16736750597207),
 .UNSPECIFIED.);
#373=B_SPLINE_CURVE_WITH_KNOTS('',3,(#13811,#13812,#13813,#13814,#13815,
#13816,#13817,#13818,#13819,#13820,#13821,#13822,#13823,#13824,#13825,#13826,
#13827,#13828,#13829,#13830,#13831,#13832),.UNSPECIFIED.,.F.,.F.,(4,2,2,
2,2,2,2,2,2,2,4),(0.0789094028588958,0.210573405340968,0.315860108011452,
0.421146810681936,0.522142632548711,0.623138454415486,0.72413427628226,
0.825130098149035,0.930416800819519,1.03570350349,1.16736750597208),
 .UNSPECIFIED.);
#374=B_SPLINE_CURVE_WITH_KNOTS('',3,(#13841,#13842,#13843,#13844,#13845,
#13846,#13847,#13848,#13849,#13850,#13851,#13852,#13853,#13854,#13855,#13856,
#13857,#13858,#13859,#13860,#13861,#13862),.UNSPECIFIED.,.F.,.F.,(4,2,2,
2,2,2,2,2,2,2,4),(0.0789094028588958,0.210573405340968,0.315860108011452,
0.421146810681936,0.522142632548711,0.623138454415485,0.72413427628226,
0.825130098149035,0.930416800819519,1.03570350349,1.16736750597208),
 .UNSPECIFIED.);
#375=B_SPLINE_CURVE_WITH_KNOTS('',3,(#14158,#14159,#14160,#14161,#14162,
#14163,#14164,#14165,#14166,#14167),.UNSPECIFIED.,.F.,.F.,(4,2,2,2,4),(0.818088904349174,
0.878131747417166,0.957937926194037,1.03774410497091,1.0977869480389),
 .UNSPECIFIED.);
#376=B_SPLINE_CURVE_WITH_KNOTS('',3,(#14173,#14174,#14175,#14176,#14177,
#14178,#14179,#14180,#14181,#14182,#14183,#14184,#14185,#14186,#14187,#14188,
#14189,#14190),.UNSPECIFIED.,.F.,.F.,(4,2,2,2,2,2,2,2,4),(0.,0.0793616477694787,
0.158723295538957,0.238079516586307,0.317435737633657,0.396791958681006,
0.476148179728356,0.555509827497835,0.634871475267313),.UNSPECIFIED.);
#377=B_SPLINE_CURVE_WITH_KNOTS('',3,(#14191,#14192,#14193,#14194,#14195,
#14196,#14197,#14198,#14199,#14200,#14201,#14202,#14203,#14204,#14205,#14206,
#14207,#14208),.UNSPECIFIED.,.F.,.F.,(4,2,2,2,2,2,2,2,4),(0.634871475267313,
0.714233123036792,0.793594770806271,0.87295099185362,0.95230721290097,1.03166343394832,
1.11101965499567,1.19038130276515,1.26974295053463),.UNSPECIFIED.);
#378=B_SPLINE_CURVE_WITH_KNOTS('',3,(#14211,#14212,#14213,#14214,#14215,
#14216,#14217,#14218,#14219,#14220),.UNSPECIFIED.,.F.,.F.,(4,2,2,2,4),(0.179463620219816,
0.239506463287808,0.319312642064679,0.39911882084155,0.459161663909542),
 .UNSPECIFIED.);
#379=B_SPLINE_CURVE_WITH_KNOTS('',3,(#14245,#14246,#14247,#14248,#14249,
#14250,#14251,#14252,#14253,#14254),.UNSPECIFIED.,.F.,.F.,(4,2,2,2,4),(0.818088904349175,
0.878131747417166,0.957937926194037,1.03774410497091,1.0977869480389),
 .UNSPECIFIED.);
#380=B_SPLINE_CURVE_WITH_KNOTS('',3,(#14260,#14261,#14262,#14263,#14264,
#14265,#14266,#14267,#14268,#14269,#14270,#14271,#14272,#14273,#14274,#14275,
#14276,#14277),.UNSPECIFIED.,.F.,.F.,(4,2,2,2,2,2,2,2,4),(0.,0.0793616477694787,
0.158723295538957,0.238079516586307,0.317435737633657,0.396791958681006,
0.476148179728356,0.555509827497835,0.634871475267313),.UNSPECIFIED.);
#381=B_SPLINE_CURVE_WITH_KNOTS('',3,(#14278,#14279,#14280,#14281,#14282,
#14283,#14284,#14285,#14286,#14287,#14288,#14289,#14290,#14291,#14292,#14293,
#14294,#14295),.UNSPECIFIED.,.F.,.F.,(4,2,2,2,2,2,2,2,4),(0.634871475267313,
0.714233123036792,0.793594770806271,0.87295099185362,0.95230721290097,1.03166343394832,
1.11101965499567,1.19038130276515,1.26974295053463),.UNSPECIFIED.);
#382=B_SPLINE_CURVE_WITH_KNOTS('',3,(#14298,#14299,#14300,#14301,#14302,
#14303,#14304,#14305,#14306,#14307),.UNSPECIFIED.,.F.,.F.,(4,2,2,2,4),(0.179463620219817,
0.239506463287808,0.319312642064679,0.39911882084155,0.459161663909542),
 .UNSPECIFIED.);
#383=B_SPLINE_CURVE_WITH_KNOTS('',3,(#14362,#14363,#14364,#14365,#14366,
#14367,#14368,#14369,#14370,#14371,#14372,#14373,#14374,#14375),
 .UNSPECIFIED.,.F.,.F.,(4,2,2,2,2,2,4),(0.75600573798702,0.793568827564647,
0.872922520054202,0.952276212543757,1.03162990503331,1.11098359752287,1.14854668710049),
 .UNSPECIFIED.);
#384=B_SPLINE_CURVE_WITH_KNOTS('',3,(#14381,#14382,#14383,#14384,#14385,
#14386,#14387,#14388,#14389,#14390,#14391,#14392,#14393,#14394,#14395,#14396,
#14397,#14398),.UNSPECIFIED.,.F.,.F.,(4,2,2,2,2,2,2,2,4),(0.,0.079216580773363,
0.158433161546726,0.23764869707457,0.316864232602414,0.396079768130259,
0.475295303658103,0.554511884431466,0.633728465204829),.UNSPECIFIED.);
#385=B_SPLINE_CURVE_WITH_KNOTS('',3,(#14399,#14400,#14401,#14402,#14403,
#14404,#14405,#14406,#14407,#14408,#14409,#14410,#14411,#14412,#14413,#14414,
#14415,#14416),.UNSPECIFIED.,.F.,.F.,(4,2,2,2,2,2,2,2,4),(0.633728465204829,
0.712945045978192,0.792161626751555,0.871377162279399,0.950592697807243,
1.02980823333509,1.10902376886293,1.18824034963629,1.26745693040966),
 .UNSPECIFIED.);
#386=B_SPLINE_CURVE_WITH_KNOTS('',3,(#14419,#14420,#14421,#14422,#14423,
#14424,#14425,#14426,#14427,#14428,#14429,#14430,#14431,#14432),
 .UNSPECIFIED.,.F.,.F.,(4,2,2,2,2,2,4),(0.121154929624515,0.158718019202143,
0.238071711691697,0.317425404181252,0.396779096670807,0.476132789160362,
0.513695878737989),.UNSPECIFIED.);
#387=B_SPLINE_CURVE_WITH_KNOTS('',3,(#14457,#14458,#14459,#14460,#14461,
#14462,#14463,#14464,#14465,#14466,#14467,#14468,#14469,#14470),
 .UNSPECIFIED.,.F.,.F.,(4,2,2,2,2,2,4),(0.75600573798702,0.793568827564647,
0.872922520054202,0.952276212543757,1.03162990503331,1.11098359752287,1.14854668710049),
 .UNSPECIFIED.);
#388=B_SPLINE_CURVE_WITH_KNOTS('',3,(#14476,#14477,#14478,#14479,#14480,
#14481,#14482,#14483,#14484,#14485,#14486,#14487,#14488,#14489,#14490,#14491,
#14492,#14493),.UNSPECIFIED.,.F.,.F.,(4,2,2,2,2,2,2,2,4),(0.,0.079216580773363,
0.158433161546726,0.23764869707457,0.316864232602414,0.396079768130259,
0.475295303658103,0.554511884431466,0.633728465204829),.UNSPECIFIED.);
#389=B_SPLINE_CURVE_WITH_KNOTS('',3,(#14494,#14495,#14496,#14497,#14498,
#14499,#14500,#14501,#14502,#14503,#14504,#14505,#14506,#14507,#14508,#14509,
#14510,#14511),.UNSPECIFIED.,.F.,.F.,(4,2,2,2,2,2,2,2,4),(0.633728465204829,
0.712945045978192,0.792161626751555,0.871377162279399,0.950592697807243,
1.02980823333509,1.10902376886293,1.18824034963629,1.26745693040966),
 .UNSPECIFIED.);
#390=B_SPLINE_CURVE_WITH_KNOTS('',3,(#14514,#14515,#14516,#14517,#14518,
#14519,#14520,#14521,#14522,#14523,#14524,#14525,#14526,#14527),
 .UNSPECIFIED.,.F.,.F.,(4,2,2,2,2,2,4),(0.121154929624516,0.158718019202143,
0.238071711691697,0.317425404181252,0.396779096670807,0.476132789160362,
0.513695878737989),.UNSPECIFIED.);
#391=B_SPLINE_CURVE_WITH_KNOTS('',3,(#14552,#14553,#14554,#14555,#14556,
#14557,#14558,#14559,#14560,#14561),.UNSPECIFIED.,.F.,.F.,(4,2,2,2,4),(0.847831445683407,
0.87827457693095,0.958092875386316,1.03791117384168,1.06835430508922),
 .UNSPECIFIED.);
#392=B_SPLINE_CURVE_WITH_KNOTS('',3,(#14567,#14568,#14569,#14570,#14571,
#14572,#14573,#14574,#14575,#14576,#14577,#14578,#14579,#14580,#14581,#14582,
#14583,#14584),.UNSPECIFIED.,.F.,.F.,(4,2,2,2,2,2,2,2,4),(0.,0.0792165807733633,
0.158433161546727,0.237648697074571,0.316864232602415,0.396079768130259,
0.475295303658104,0.554511884431467,0.63372846520483),.UNSPECIFIED.);
#393=B_SPLINE_CURVE_WITH_KNOTS('',3,(#14585,#14586,#14587,#14588,#14589,
#14590,#14591,#14592,#14593,#14594,#14595,#14596,#14597,#14598,#14599,#14600,
#14601,#14602),.UNSPECIFIED.,.F.,.F.,(4,2,2,2,2,2,2,2,4),(0.63372846520483,
0.712945045978194,0.792161626751557,0.871377162279401,0.950592697807245,
1.02980823333509,1.10902376886293,1.1882403496363,1.26745693040966),
 .UNSPECIFIED.);
#394=B_SPLINE_CURVE_WITH_KNOTS('',3,(#14605,#14606,#14607,#14608,#14609,
#14610,#14611,#14612,#14613,#14614),.UNSPECIFIED.,.F.,.F.,(4,2,2,2,4),(0.20910286209253,
0.239545993340073,0.319364291795439,0.399182590250804,0.429625721498348),
 .UNSPECIFIED.);
#395=SPHERICAL_SURFACE('',#8664,0.29765);
#396=SPHERICAL_SURFACE('',#8666,0.29765);
#397=SPHERICAL_SURFACE('',#8668,0.29765);
#398=SPHERICAL_SURFACE('',#8670,0.29765);
#399=SPHERICAL_SURFACE('',#8672,0.29765);
#400=SPHERICAL_SURFACE('',#8674,0.29765);
#401=SPHERICAL_SURFACE('',#8676,0.29765);
#402=SPHERICAL_SURFACE('',#8679,0.309556);
#403=SPHERICAL_SURFACE('',#8695,0.309556);
#404=SPHERICAL_SURFACE('',#8700,0.309556);
#405=SPHERICAL_SURFACE('',#8706,0.309556);
#406=SPHERICAL_SURFACE('',#8711,0.309556);
#407=SPHERICAL_SURFACE('',#8716,0.309556);
#408=SPHERICAL_SURFACE('',#8724,0.309556);
#409=SPHERICAL_SURFACE('',#8792,0.3969);
#410=SPHERICAL_SURFACE('',#8794,0.3969);
#411=SPHERICAL_SURFACE('',#8796,0.3969);
#412=SPHERICAL_SURFACE('',#8798,0.3969);
#413=SPHERICAL_SURFACE('',#8800,0.3969);
#414=SPHERICAL_SURFACE('',#8802,0.3969);
#415=SPHERICAL_SURFACE('',#8804,0.3969);
#416=SPHERICAL_SURFACE('',#8806,0.3969);
#417=SPHERICAL_SURFACE('',#8809,0.412776);
#418=SPHERICAL_SURFACE('',#8825,0.412776);
#419=SPHERICAL_SURFACE('',#8830,0.412776);
#420=SPHERICAL_SURFACE('',#8835,0.412776);
#421=SPHERICAL_SURFACE('',#8840,0.412776);
#422=SPHERICAL_SURFACE('',#8845,0.412776);
#423=SPHERICAL_SURFACE('',#8850,0.412776);
#424=SPHERICAL_SURFACE('',#8858,0.412776);
#425=TOROIDAL_SURFACE('',#8624,1.1,0.309556);
#426=TOROIDAL_SURFACE('',#8644,1.1,0.309556);
#427=TOROIDAL_SURFACE('',#8752,1.675,0.412776);
#428=TOROIDAL_SURFACE('',#8772,1.675,0.412776);
#429=CONICAL_SURFACE('',#8611,0.475,0.785398163397449);
#430=CONICAL_SURFACE('',#8615,0.485,0.785398163397448);
#431=CONICAL_SURFACE('',#8619,0.31,0.463647609000806);
#432=CONICAL_SURFACE('',#8635,0.63,0.785398163397448);
#433=CONICAL_SURFACE('',#8642,0.63,0.785398163397448);
#434=CONICAL_SURFACE('',#8655,1.57,0.785398163397449);
#435=CONICAL_SURFACE('',#8659,1.57,0.785398163397449);
#436=CONICAL_SURFACE('',#8763,1.05,0.785398163397449);
#437=CONICAL_SURFACE('',#8770,1.05,0.785398163397449);
#438=CONICAL_SURFACE('',#8783,2.3,0.785398163397449);
#439=CONICAL_SURFACE('',#8787,2.3,0.785398163397449);
#440=CONICAL_SURFACE('',#8887,0.4,0.785398163397448);
#441=CONICAL_SURFACE('',#8891,0.41,0.785398163397448);
#442=CONICAL_SURFACE('',#8895,0.26,0.463647609000806);
#443=CONICAL_SURFACE('',#8899,0.225,0.785398163397448);
#444=CONICAL_SURFACE('',#8923,0.325,0.785398163397448);
#445=CONICAL_SURFACE('',#8927,0.335,0.785398163397448);
#446=CONICAL_SURFACE('',#8931,0.21,0.463647609000806);
#447=CONICAL_SURFACE('',#9142,0.235,0.785398163397448);
#448=CONICAL_SURFACE('',#9146,0.2125,0.785398163397448);
#449=ORIENTED_CLOSED_SHELL('',*,#7670,.F.);
#450=ORIENTED_CLOSED_SHELL('',*,#7698,.F.);
#451=ORIENTED_CLOSED_SHELL('',*,#7699,.F.);
#452=BREP_WITH_VOIDS('Body1',#7671,(#449));
#453=BREP_WITH_VOIDS('Body1',#7697,(#450));
#454=BREP_WITH_VOIDS('Body1',#7700,(#451));
#455=ELLIPSE('',#8204,1.22383731671239,0.6);
#456=ELLIPSE('',#8205,1.22383731671239,0.6);
#457=ELLIPSE('',#8213,1.22383731671239,0.6);
#458=ELLIPSE('',#8300,1.22383731671239,0.6);
#459=ELLIPSE('',#8301,1.22383731671239,0.6);
#460=ELLIPSE('',#8309,1.22383731671239,0.6);
#461=SHAPE_REPRESENTATION_RELATIONSHIP('SRR','None',#15000,#500);
#462=SHAPE_REPRESENTATION_RELATIONSHIP('SRR','None',#15001,#501);
#463=SHAPE_REPRESENTATION_RELATIONSHIP('SRR','None',#15002,#502);
#464=SHAPE_REPRESENTATION_RELATIONSHIP('SRR','None',#15003,#503);
#465=SHAPE_REPRESENTATION_RELATIONSHIP('SRR','None',#15004,#504);
#466=SHAPE_REPRESENTATION_RELATIONSHIP('SRR','None',#15005,#505);
#467=SHAPE_REPRESENTATION_RELATIONSHIP('SRR','None',#15006,#506);
#468=SHAPE_REPRESENTATION_RELATIONSHIP('SRR','None',#15007,#507);
#469=SHAPE_REPRESENTATION_RELATIONSHIP('SRR','None',#15008,#508);
#470=SHAPE_REPRESENTATION_RELATIONSHIP('SRR','None',#15009,#509);
#471=SHAPE_REPRESENTATION_RELATIONSHIP('SRR','None',#15010,#510);
#472=SHAPE_REPRESENTATION_RELATIONSHIP('SRR','None',#15011,#511);
#473=SHAPE_REPRESENTATION_RELATIONSHIP('SRR','None',#15012,#512);
#474=SHAPE_REPRESENTATION_RELATIONSHIP('SRR','None',#15013,#513);
#475=SHAPE_REPRESENTATION_RELATIONSHIP('SRR','None',#15014,#514);
#476=SHAPE_REPRESENTATION_RELATIONSHIP('SRR','None',#15015,#515);
#477=SHAPE_REPRESENTATION_RELATIONSHIP('SRR','None',#15017,#516);
#478=SHAPE_REPRESENTATION_RELATIONSHIP('SRR','None',#15018,#517);
#479=SHAPE_REPRESENTATION_RELATIONSHIP('SRR','None',#15019,#518);
#480=SHAPE_REPRESENTATION_RELATIONSHIP('SRR','None',#15020,#519);
#481=SHAPE_REPRESENTATION_RELATIONSHIP('SRR','None',#15021,#520);
#482=SHAPE_REPRESENTATION_RELATIONSHIP('SRR','None',#15023,#521);
#483=SHAPE_REPRESENTATION_RELATIONSHIP('SRR','None',#15024,#522);
#484=SHAPE_REPRESENTATION_RELATIONSHIP('SRR','None',#15025,#523);
#485=SHAPE_REPRESENTATION_RELATIONSHIP('SRR','None',#15026,#524);
#486=SHAPE_REPRESENTATION_RELATIONSHIP('SRR','None',#15027,#525);
#487=SHAPE_REPRESENTATION_RELATIONSHIP('SRR','None',#15028,#526);
#488=SHAPE_REPRESENTATION_RELATIONSHIP('SRR','None',#15029,#527);
#489=SHAPE_REPRESENTATION_RELATIONSHIP('SRR','None',#15031,#528);
#490=SHAPE_REPRESENTATION_RELATIONSHIP('SRR','None',#15032,#529);
#491=SHAPE_REPRESENTATION_RELATIONSHIP('SRR','None',#15033,#530);
#492=SHAPE_REPRESENTATION_RELATIONSHIP('SRR','None',#15034,#531);
#493=SHAPE_REPRESENTATION_RELATIONSHIP('SRR','None',#15035,#532);
#494=SHAPE_REPRESENTATION_RELATIONSHIP('SRR','None',#15036,#533);
#495=SHAPE_REPRESENTATION_RELATIONSHIP('SRR','None',#15037,#534);
#496=SHAPE_REPRESENTATION_RELATIONSHIP('SRR','None',#15038,#535);
#497=SHAPE_REPRESENTATION_RELATIONSHIP('SRR','None',#15039,#536);
#498=SHAPE_REPRESENTATION_RELATIONSHIP('SRR','None',#15040,#537);
#499=SHAPE_REPRESENTATION_RELATIONSHIP('SRR','None',#15041,#538);
#500=ADVANCED_BREP_SHAPE_REPRESENTATION('',(#593),#14780);
#501=ADVANCED_BREP_SHAPE_REPRESENTATION('',(#594),#14781);
#502=ADVANCED_BREP_SHAPE_REPRESENTATION('',(#595),#14782);
#503=ADVANCED_BREP_SHAPE_REPRESENTATION('',(#596),#14783);
#504=ADVANCED_BREP_SHAPE_REPRESENTATION('',(#597),#14784);
#505=ADVANCED_BREP_SHAPE_REPRESENTATION('',(#598),#14785);
#506=ADVANCED_BREP_SHAPE_REPRESENTATION('',(#599),#14786);
#507=ADVANCED_BREP_SHAPE_REPRESENTATION('',(#600),#14787);
#508=ADVANCED_BREP_SHAPE_REPRESENTATION('',(#601),#14788);
#509=ADVANCED_BREP_SHAPE_REPRESENTATION('',(#602),#14789);
#510=ADVANCED_BREP_SHAPE_REPRESENTATION('',(#603),#14790);
#511=ADVANCED_BREP_SHAPE_REPRESENTATION('',(#604),#14791);
#512=ADVANCED_BREP_SHAPE_REPRESENTATION('',(#605),#14792);
#513=ADVANCED_BREP_SHAPE_REPRESENTATION('',(#606),#14793);
#514=ADVANCED_BREP_SHAPE_REPRESENTATION('',(#607),#14794);
#515=ADVANCED_BREP_SHAPE_REPRESENTATION('',(#452),#14795);
#516=ADVANCED_BREP_SHAPE_REPRESENTATION('',(#608),#14797);
#517=ADVANCED_BREP_SHAPE_REPRESENTATION('',(#609),#14798);
#518=ADVANCED_BREP_SHAPE_REPRESENTATION('',(#610,#611,#612,#613,#614,#615,
#616),#14799);
#519=ADVANCED_BREP_SHAPE_REPRESENTATION('',(#617),#14800);
#520=ADVANCED_BREP_SHAPE_REPRESENTATION('',(#618,#619),#14801);
#521=ADVANCED_BREP_SHAPE_REPRESENTATION('',(#620),#14803);
#522=ADVANCED_BREP_SHAPE_REPRESENTATION('',(#621),#14804);
#523=ADVANCED_BREP_SHAPE_REPRESENTATION('',(#622,#623,#624,#625,#626,#627,
#628,#629),#14805);
#524=ADVANCED_BREP_SHAPE_REPRESENTATION('',(#630),#14806);
#525=ADVANCED_BREP_SHAPE_REPRESENTATION('',(#631,#632),#14807);
#526=ADVANCED_BREP_SHAPE_REPRESENTATION('',(#453),#14808);
#527=ADVANCED_BREP_SHAPE_REPRESENTATION('',(#454),#14809);
#528=ADVANCED_BREP_SHAPE_REPRESENTATION('',(#633),#14811);
#529=ADVANCED_BREP_SHAPE_REPRESENTATION('',(#634),#14812);
#530=ADVANCED_BREP_SHAPE_REPRESENTATION('',(#635),#14813);
#531=ADVANCED_BREP_SHAPE_REPRESENTATION('',(#636),#14814);
#532=ADVANCED_BREP_SHAPE_REPRESENTATION('',(#637),#14815);
#533=ADVANCED_BREP_SHAPE_REPRESENTATION('',(#638),#14816);
#534=ADVANCED_BREP_SHAPE_REPRESENTATION('',(#639),#14817);
#535=ADVANCED_BREP_SHAPE_REPRESENTATION('',(#640),#14818);
#536=ADVANCED_BREP_SHAPE_REPRESENTATION('',(#641),#14819);
#537=ADVANCED_BREP_SHAPE_REPRESENTATION('',(#642),#14820);
#538=ADVANCED_BREP_SHAPE_REPRESENTATION('',(#643),#14821);
#539=STYLED_ITEM('',(#15263),#593);
#540=STYLED_ITEM('',(#15263),#594);
#541=STYLED_ITEM('',(#15277),#595);
#542=STYLED_ITEM('',(#15277),#596);
#543=STYLED_ITEM('',(#15263),#597);
#544=STYLED_ITEM('',(#15277),#598);
#545=STYLED_ITEM('',(#15277),#599);
#546=STYLED_ITEM('',(#15263),#600);
#547=STYLED_ITEM('',(#15284),#601);
#548=STYLED_ITEM('',(#15284),#602);
#549=STYLED_ITEM('',(#15298),#603);
#550=STYLED_ITEM('',(#15270),#604);
#551=STYLED_ITEM('',(#15263),#605);
#552=STYLED_ITEM('',(#15277),#606);
#553=STYLED_ITEM('',(#15277),#607);
#554=STYLED_ITEM('',(#15291),#452);
#555=STYLED_ITEM('',(#15284),#608);
#556=STYLED_ITEM('',(#15284),#609);
#557=STYLED_ITEM('',(#15284),#610);
#558=STYLED_ITEM('',(#15284),#611);
#559=STYLED_ITEM('',(#15284),#612);
#560=STYLED_ITEM('',(#15284),#613);
#561=STYLED_ITEM('',(#15284),#614);
#562=STYLED_ITEM('',(#15284),#615);
#563=STYLED_ITEM('',(#15284),#616);
#564=STYLED_ITEM('',(#15284),#617);
#565=STYLED_ITEM('',(#15284),#618);
#566=STYLED_ITEM('',(#15284),#619);
#567=STYLED_ITEM('',(#15284),#620);
#568=STYLED_ITEM('',(#15284),#621);
#569=STYLED_ITEM('',(#15284),#622);
#570=STYLED_ITEM('',(#15284),#623);
#571=STYLED_ITEM('',(#15284),#624);
#572=STYLED_ITEM('',(#15284),#625);
#573=STYLED_ITEM('',(#15284),#626);
#574=STYLED_ITEM('',(#15284),#627);
#575=STYLED_ITEM('',(#15284),#628);
#576=STYLED_ITEM('',(#15284),#629);
#577=STYLED_ITEM('',(#15284),#630);
#578=STYLED_ITEM('',(#15284),#631);
#579=STYLED_ITEM('',(#15284),#632);
#580=STYLED_ITEM('',(#15291),#453);
#581=STYLED_ITEM('',(#15291),#454);
#582=STYLED_ITEM('',(#15277),#633);
#583=STYLED_ITEM('',(#15298),#634);
#584=STYLED_ITEM('',(#15298),#635);
#585=STYLED_ITEM('',(#15277),#636);
#586=STYLED_ITEM('',(#15277),#637);
#587=STYLED_ITEM('',(#15277),#638);
#588=STYLED_ITEM('',(#15277),#639);
#589=STYLED_ITEM('',(#15284),#640);
#590=STYLED_ITEM('',(#15284),#641);
#591=STYLED_ITEM('',(#15277),#642);
#592=STYLED_ITEM('',(#15291),#643);
#593=MANIFOLD_SOLID_BREP('Body1',#7655);
#594=MANIFOLD_SOLID_BREP('Body1',#7656);
#595=MANIFOLD_SOLID_BREP('Body1',#7657);
#596=MANIFOLD_SOLID_BREP('Body1',#7658);
#597=MANIFOLD_SOLID_BREP('Body1',#7659);
#598=MANIFOLD_SOLID_BREP('Body1',#7660);
#599=MANIFOLD_SOLID_BREP('Body1',#7661);
#600=MANIFOLD_SOLID_BREP('Body1',#7662);
#601=MANIFOLD_SOLID_BREP('Body1',#7663);
#602=MANIFOLD_SOLID_BREP('Body1',#7664);
#603=MANIFOLD_SOLID_BREP('Body1',#7665);
#604=MANIFOLD_SOLID_BREP('Body1',#7666);
#605=MANIFOLD_SOLID_BREP('Body1',#7667);
#606=MANIFOLD_SOLID_BREP('Body1',#7668);
#607=MANIFOLD_SOLID_BREP('Body1',#7669);
#608=MANIFOLD_SOLID_BREP('Body1',#7672);
#609=MANIFOLD_SOLID_BREP('Body1',#7673);
#610=MANIFOLD_SOLID_BREP('Body1',#7674);
#611=MANIFOLD_SOLID_BREP('Body2',#7675);
#612=MANIFOLD_SOLID_BREP('Body3',#7676);
#613=MANIFOLD_SOLID_BREP('Body4',#7677);
#614=MANIFOLD_SOLID_BREP('Body5',#7678);
#615=MANIFOLD_SOLID_BREP('Body6',#7679);
#616=MANIFOLD_SOLID_BREP('Body7',#7680);
#617=MANIFOLD_SOLID_BREP('Continuous crown cage',#7681);
#618=MANIFOLD_SOLID_BREP('Body1',#7682);
#619=MANIFOLD_SOLID_BREP('Body2',#7683);
#620=MANIFOLD_SOLID_BREP('Body1',#7684);
#621=MANIFOLD_SOLID_BREP('Body1',#7685);
#622=MANIFOLD_SOLID_BREP('Body1',#7686);
#623=MANIFOLD_SOLID_BREP('Body2',#7687);
#624=MANIFOLD_SOLID_BREP('Body3',#7688);
#625=MANIFOLD_SOLID_BREP('Body4',#7689);
#626=MANIFOLD_SOLID_BREP('Body5',#7690);
#627=MANIFOLD_SOLID_BREP('Body6',#7691);
#628=MANIFOLD_SOLID_BREP('Body7',#7692);
#629=MANIFOLD_SOLID_BREP('Body8',#7693);
#630=MANIFOLD_SOLID_BREP('Continuous crown cage',#7694);
#631=MANIFOLD_SOLID_BREP('Body1',#7695);
#632=MANIFOLD_SOLID_BREP('Body2',#7696);
#633=MANIFOLD_SOLID_BREP('Body1',#7701);
#634=MANIFOLD_SOLID_BREP('Body1',#7702);
#635=MANIFOLD_SOLID_BREP('Body1',#7703);
#636=MANIFOLD_SOLID_BREP('Body1',#7704);
#637=MANIFOLD_SOLID_BREP('Body1',#7705);
#638=MANIFOLD_SOLID_BREP('Body1',#7706);
#639=MANIFOLD_SOLID_BREP('Body1',#7707);
#640=MANIFOLD_SOLID_BREP('Body1',#7708);
#641=MANIFOLD_SOLID_BREP('Body1',#7709);
#642=MANIFOLD_SOLID_BREP('Body1',#7710);
#643=MANIFOLD_SOLID_BREP('Body1',#7711);
#644=FACE_BOUND('',#1561,.T.);
#645=FACE_BOUND('',#1562,.T.);
#646=FACE_BOUND('',#1563,.T.);
#647=FACE_BOUND('',#1564,.T.);
#648=FACE_BOUND('',#1565,.T.);
#649=FACE_BOUND('',#1566,.T.);
#650=FACE_BOUND('',#1567,.T.);
#651=FACE_BOUND('',#1568,.T.);
#652=FACE_BOUND('',#1569,.T.);
#653=FACE_BOUND('',#1570,.T.);
#654=FACE_BOUND('',#1571,.T.);
#655=FACE_BOUND('',#1572,.T.);
#656=FACE_BOUND('',#1574,.T.);
#657=FACE_BOUND('',#1575,.T.);
#658=FACE_BOUND('',#1576,.T.);
#659=FACE_BOUND('',#1577,.T.);
#660=FACE_BOUND('',#1578,.T.);
#661=FACE_BOUND('',#1579,.T.);
#662=FACE_BOUND('',#1580,.T.);
#663=FACE_BOUND('',#1581,.T.);
#664=FACE_BOUND('',#1582,.T.);
#665=FACE_BOUND('',#1583,.T.);
#666=FACE_BOUND('',#1584,.T.);
#667=FACE_BOUND('',#1585,.T.);
#668=FACE_BOUND('',#1593,.T.);
#669=FACE_BOUND('',#1597,.T.);
#670=FACE_BOUND('',#1601,.T.);
#671=FACE_BOUND('',#1603,.T.);
#672=FACE_BOUND('',#1606,.T.);
#673=FACE_BOUND('',#1607,.T.);
#674=FACE_BOUND('',#1610,.T.);
#675=FACE_BOUND('',#1611,.T.);
#676=FACE_BOUND('',#1612,.T.);
#677=FACE_BOUND('',#1613,.T.);
#678=FACE_BOUND('',#1614,.T.);
#679=FACE_BOUND('',#1618,.T.);
#680=FACE_BOUND('',#1619,.T.);
#681=FACE_BOUND('',#1620,.T.);
#682=FACE_BOUND('',#1621,.T.);
#683=FACE_BOUND('',#1622,.T.);
#684=FACE_BOUND('',#1629,.T.);
#685=FACE_BOUND('',#1633,.T.);
#686=FACE_BOUND('',#1634,.T.);
#687=FACE_BOUND('',#1635,.T.);
#688=FACE_BOUND('',#1636,.T.);
#689=FACE_BOUND('',#1637,.T.);
#690=FACE_BOUND('',#1639,.T.);
#691=FACE_BOUND('',#1640,.T.);
#692=FACE_BOUND('',#1641,.T.);
#693=FACE_BOUND('',#1642,.T.);
#694=FACE_BOUND('',#1643,.T.);
#695=FACE_BOUND('',#1650,.T.);
#696=FACE_BOUND('',#1654,.T.);
#697=FACE_BOUND('',#1655,.T.);
#698=FACE_BOUND('',#1656,.T.);
#699=FACE_BOUND('',#1657,.T.);
#700=FACE_BOUND('',#1658,.T.);
#701=FACE_BOUND('',#1660,.T.);
#702=FACE_BOUND('',#1661,.T.);
#703=FACE_BOUND('',#1662,.T.);
#704=FACE_BOUND('',#1663,.T.);
#705=FACE_BOUND('',#1664,.T.);
#706=FACE_BOUND('',#1672,.T.);
#707=FACE_BOUND('',#1676,.T.);
#708=FACE_BOUND('',#1680,.T.);
#709=FACE_BOUND('',#1682,.T.);
#710=FACE_BOUND('',#1685,.T.);
#711=FACE_BOUND('',#1686,.T.);
#712=FACE_BOUND('',#1689,.T.);
#713=FACE_BOUND('',#1690,.T.);
#714=FACE_BOUND('',#1691,.T.);
#715=FACE_BOUND('',#1692,.T.);
#716=FACE_BOUND('',#1693,.T.);
#717=FACE_BOUND('',#1697,.T.);
#718=FACE_BOUND('',#1698,.T.);
#719=FACE_BOUND('',#1699,.T.);
#720=FACE_BOUND('',#1700,.T.);
#721=FACE_BOUND('',#1701,.T.);
#722=FACE_BOUND('',#1708,.T.);
#723=FACE_BOUND('',#1712,.T.);
#724=FACE_BOUND('',#1713,.T.);
#725=FACE_BOUND('',#1714,.T.);
#726=FACE_BOUND('',#1715,.T.);
#727=FACE_BOUND('',#1716,.T.);
#728=FACE_BOUND('',#1718,.T.);
#729=FACE_BOUND('',#1719,.T.);
#730=FACE_BOUND('',#1720,.T.);
#731=FACE_BOUND('',#1721,.T.);
#732=FACE_BOUND('',#1722,.T.);
#733=FACE_BOUND('',#1729,.T.);
#734=FACE_BOUND('',#1733,.T.);
#735=FACE_BOUND('',#1734,.T.);
#736=FACE_BOUND('',#1735,.T.);
#737=FACE_BOUND('',#1736,.T.);
#738=FACE_BOUND('',#1737,.T.);
#739=FACE_BOUND('',#1739,.T.);
#740=FACE_BOUND('',#1740,.T.);
#741=FACE_BOUND('',#1741,.T.);
#742=FACE_BOUND('',#1742,.T.);
#743=FACE_BOUND('',#1743,.T.);
#744=FACE_BOUND('',#1755,.T.);
#745=FACE_BOUND('',#1757,.T.);
#746=FACE_BOUND('',#1758,.T.);
#747=FACE_BOUND('',#1759,.T.);
#748=FACE_BOUND('',#1760,.T.);
#749=FACE_BOUND('',#1761,.T.);
#750=FACE_BOUND('',#1763,.T.);
#751=FACE_BOUND('',#1764,.T.);
#752=FACE_BOUND('',#1765,.T.);
#753=FACE_BOUND('',#1766,.T.);
#754=FACE_BOUND('',#1767,.T.);
#755=FACE_BOUND('',#1774,.T.);
#756=FACE_BOUND('',#1778,.T.);
#757=FACE_BOUND('',#1779,.T.);
#758=FACE_BOUND('',#1780,.T.);
#759=FACE_BOUND('',#1781,.T.);
#760=FACE_BOUND('',#1782,.T.);
#761=FACE_BOUND('',#1784,.T.);
#762=FACE_BOUND('',#1785,.T.);
#763=FACE_BOUND('',#1786,.T.);
#764=FACE_BOUND('',#1787,.T.);
#765=FACE_BOUND('',#1788,.T.);
#766=FACE_BOUND('',#1795,.T.);
#767=FACE_BOUND('',#1799,.T.);
#768=FACE_BOUND('',#1800,.T.);
#769=FACE_BOUND('',#1801,.T.);
#770=FACE_BOUND('',#1802,.T.);
#771=FACE_BOUND('',#1803,.T.);
#772=FACE_BOUND('',#1805,.T.);
#773=FACE_BOUND('',#1806,.T.);
#774=FACE_BOUND('',#1807,.T.);
#775=FACE_BOUND('',#1808,.T.);
#776=FACE_BOUND('',#1809,.T.);
#777=FACE_BOUND('',#1816,.T.);
#778=FACE_BOUND('',#1819,.T.);
#779=FACE_BOUND('',#1822,.T.);
#780=FACE_BOUND('',#1825,.T.);
#781=FACE_BOUND('',#1835,.T.);
#782=FACE_BOUND('',#1836,.T.);
#783=FACE_BOUND('',#1837,.T.);
#784=FACE_BOUND('',#1838,.T.);
#785=FACE_BOUND('',#1839,.T.);
#786=FACE_BOUND('',#1840,.T.);
#787=FACE_BOUND('',#1842,.T.);
#788=FACE_BOUND('',#1843,.T.);
#789=FACE_BOUND('',#1844,.T.);
#790=FACE_BOUND('',#1845,.T.);
#791=FACE_BOUND('',#1849,.T.);
#792=FACE_BOUND('',#1853,.T.);
#793=FACE_BOUND('',#1860,.T.);
#794=FACE_BOUND('',#1861,.T.);
#795=FACE_BOUND('',#1864,.T.);
#796=FACE_BOUND('',#1867,.T.);
#797=FACE_BOUND('',#1873,.T.);
#798=FACE_BOUND('',#1876,.T.);
#799=FACE_BOUND('',#1882,.T.);
#800=FACE_BOUND('',#1885,.T.);
#801=FACE_BOUND('',#1891,.T.);
#802=FACE_BOUND('',#1894,.T.);
#803=FACE_BOUND('',#1904,.T.);
#804=FACE_BOUND('',#1907,.T.);
#805=FACE_BOUND('',#1909,.T.);
#806=FACE_BOUND('',#1911,.T.);
#807=FACE_BOUND('',#1914,.T.);
#808=FACE_BOUND('',#1917,.T.);
#809=FACE_BOUND('',#1918,.T.);
#810=FACE_BOUND('',#1919,.T.);
#811=FACE_BOUND('',#1920,.T.);
#812=FACE_BOUND('',#1921,.T.);
#813=FACE_BOUND('',#1948,.T.);
#814=FACE_BOUND('',#1956,.T.);
#815=FACE_BOUND('',#1959,.T.);
#816=FACE_BOUND('',#1964,.T.);
#817=FACE_BOUND('',#1969,.T.);
#818=FACE_BOUND('',#1994,.T.);
#819=FACE_BOUND('',#1997,.T.);
#820=FACE_BOUND('',#2000,.T.);
#821=FACE_BOUND('',#2003,.T.);
#822=FACE_BOUND('',#2006,.T.);
#823=FACE_BOUND('',#2013,.T.);
#824=FACE_BOUND('',#2016,.T.);
#825=FACE_BOUND('',#2021,.T.);
#826=FACE_BOUND('',#2026,.T.);
#827=FACE_BOUND('',#2054,.T.);
#828=FACE_BOUND('',#2057,.T.);
#829=FACE_BOUND('',#2060,.T.);
#830=FACE_BOUND('',#2063,.T.);
#831=FACE_BOUND('',#2066,.T.);
#832=FACE_BOUND('',#2073,.T.);
#833=FACE_BOUND('',#2100,.T.);
#834=FACE_BOUND('',#2109,.T.);
#835=FACE_BOUND('',#2111,.T.);
#836=FACE_BOUND('',#2115,.T.);
#837=FACE_BOUND('',#2117,.T.);
#838=FACE_BOUND('',#2121,.T.);
#839=FACE_BOUND('',#2123,.T.);
#840=FACE_BOUND('',#2128,.T.);
#841=FACE_BOUND('',#2130,.T.);
#842=FACE_BOUND('',#2132,.T.);
#843=FACE_BOUND('',#2134,.T.);
#844=FACE_BOUND('',#2139,.T.);
#845=FACE_BOUND('',#2141,.T.);
#846=FACE_BOUND('',#2143,.T.);
#847=FACE_BOUND('',#2145,.T.);
#848=FACE_BOUND('',#2149,.T.);
#849=FACE_BOUND('',#2151,.T.);
#850=FACE_BOUND('',#2155,.T.);
#851=FACE_BOUND('',#2157,.T.);
#852=FACE_BOUND('',#2162,.T.);
#853=FACE_BOUND('',#2164,.T.);
#854=FACE_BOUND('',#2166,.T.);
#855=FACE_BOUND('',#2168,.T.);
#856=FACE_BOUND('',#2173,.T.);
#857=FACE_BOUND('',#2175,.T.);
#858=FACE_BOUND('',#2177,.T.);
#859=FACE_BOUND('',#2179,.T.);
#860=FACE_BOUND('',#2188,.T.);
#861=FACE_BOUND('',#2189,.T.);
#862=FACE_BOUND('',#2190,.T.);
#863=FACE_BOUND('',#2191,.T.);
#864=FACE_BOUND('',#2192,.T.);
#865=FACE_BOUND('',#2195,.T.);
#866=FACE_BOUND('',#2197,.T.);
#867=FACE_BOUND('',#2199,.T.);
#868=FACE_BOUND('',#2201,.T.);
#869=FACE_BOUND('',#2202,.T.);
#870=FACE_BOUND('',#2203,.T.);
#871=FACE_BOUND('',#2204,.T.);
#872=FACE_BOUND('',#2205,.T.);
#873=FACE_BOUND('',#2214,.T.);
#874=PLANE('',#8181);
#875=PLANE('',#8182);
#876=PLANE('',#8183);
#877=PLANE('',#8184);
#878=PLANE('',#8185);
#879=PLANE('',#8186);
#880=PLANE('',#8200);
#881=PLANE('',#8206);
#882=PLANE('',#8208);
#883=PLANE('',#8214);
#884=PLANE('',#8220);
#885=PLANE('',#8221);
#886=PLANE('',#8222);
#887=PLANE('',#8223);
#888=PLANE('',#8224);
#889=PLANE('',#8225);
#890=PLANE('',#8232);
#891=PLANE('',#8249);
#892=PLANE('',#8256);
#893=PLANE('',#8257);
#894=PLANE('',#8274);
#895=PLANE('',#8281);
#896=PLANE('',#8282);
#897=PLANE('',#8296);
#898=PLANE('',#8302);
#899=PLANE('',#8304);
#900=PLANE('',#8310);
#901=PLANE('',#8316);
#902=PLANE('',#8317);
#903=PLANE('',#8318);
#904=PLANE('',#8319);
#905=PLANE('',#8320);
#906=PLANE('',#8321);
#907=PLANE('',#8328);
#908=PLANE('',#8345);
#909=PLANE('',#8352);
#910=PLANE('',#8353);
#911=PLANE('',#8370);
#912=PLANE('',#8377);
#913=PLANE('',#8378);
#914=PLANE('',#8392);
#915=PLANE('',#8393);
#916=PLANE('',#8395);
#917=PLANE('',#8397);
#918=PLANE('',#8398);
#919=PLANE('',#8405);
#920=PLANE('',#8406);
#921=PLANE('',#8423);
#922=PLANE('',#8430);
#923=PLANE('',#8431);
#924=PLANE('',#8448);
#925=PLANE('',#8455);
#926=PLANE('',#8456);
#927=PLANE('',#8461);
#928=PLANE('',#8465);
#929=PLANE('',#8469);
#930=PLANE('',#8474);
#931=PLANE('',#8479);
#932=PLANE('',#8484);
#933=PLANE('',#8494);
#934=PLANE('',#8495);
#935=PLANE('',#8496);
#936=PLANE('',#8497);
#937=PLANE('',#8498);
#938=PLANE('',#8499);
#939=PLANE('',#8507);
#940=PLANE('',#8508);
#941=PLANE('',#8509);
#942=PLANE('',#8510);
#943=PLANE('',#8511);
#944=PLANE('',#8512);
#945=PLANE('',#8513);
#946=PLANE('',#8514);
#947=PLANE('',#8515);
#948=PLANE('',#8516);
#949=PLANE('',#8521);
#950=PLANE('',#8525);
#951=PLANE('',#8529);
#952=PLANE('',#8530);
#953=PLANE('',#8534);
#954=PLANE('',#8538);
#955=PLANE('',#8542);
#956=PLANE('',#8543);
#957=PLANE('',#8547);
#958=PLANE('',#8551);
#959=PLANE('',#8555);
#960=PLANE('',#8556);
#961=PLANE('',#8560);
#962=PLANE('',#8564);
#963=PLANE('',#8568);
#964=PLANE('',#8569);
#965=PLANE('',#8570);
#966=PLANE('',#8571);
#967=PLANE('',#8572);
#968=PLANE('',#8573);
#969=PLANE('',#8574);
#970=PLANE('',#8575);
#971=PLANE('',#8576);
#972=PLANE('',#8577);
#973=PLANE('',#8578);
#974=PLANE('',#8579);
#975=PLANE('',#8580);
#976=PLANE('',#8581);
#977=PLANE('',#8582);
#978=PLANE('',#8583);
#979=PLANE('',#8585);
#980=PLANE('',#8586);
#981=PLANE('',#8587);
#982=PLANE('',#8588);
#983=PLANE('',#8589);
#984=PLANE('',#8590);
#985=PLANE('',#8592);
#986=PLANE('',#8593);
#987=PLANE('',#8594);
#988=PLANE('',#8595);
#989=PLANE('',#8596);
#990=PLANE('',#8597);
#991=PLANE('',#8599);
#992=PLANE('',#8600);
#993=PLANE('',#8601);
#994=PLANE('',#8602);
#995=PLANE('',#8603);
#996=PLANE('',#8604);
#997=PLANE('',#8605);
#998=PLANE('',#8606);
#999=PLANE('',#8607);
#1000=PLANE('',#8609);
#1001=PLANE('',#8617);
#1002=PLANE('',#8637);
#1003=PLANE('',#8640);
#1004=PLANE('',#8652);
#1005=PLANE('',#8661);
#1006=PLANE('',#8692);
#1007=PLANE('',#8697);
#1008=PLANE('',#8702);
#1009=PLANE('',#8708);
#1010=PLANE('',#8713);
#1011=PLANE('',#8722);
#1012=PLANE('',#8726);
#1013=PLANE('',#8727);
#1014=PLANE('',#8729);
#1015=PLANE('',#8734);
#1016=PLANE('',#8737);
#1017=PLANE('',#8742);
#1018=PLANE('',#8765);
#1019=PLANE('',#8768);
#1020=PLANE('',#8780);
#1021=PLANE('',#8789);
#1022=PLANE('',#8822);
#1023=PLANE('',#8827);
#1024=PLANE('',#8832);
#1025=PLANE('',#8837);
#1026=PLANE('',#8842);
#1027=PLANE('',#8847);
#1028=PLANE('',#8856);
#1029=PLANE('',#8860);
#1030=PLANE('',#8861);
#1031=PLANE('',#8863);
#1032=PLANE('',#8868);
#1033=PLANE('',#8871);
#1034=PLANE('',#8876);
#1035=PLANE('',#8885);
#1036=PLANE('',#8893);
#1037=PLANE('',#8901);
#1038=PLANE('',#8902);
#1039=PLANE('',#8903);
#1040=PLANE('',#8904);
#1041=PLANE('',#8905);
#1042=PLANE('',#8906);
#1043=PLANE('',#8907);
#1044=PLANE('',#8908);
#1045=PLANE('',#8909);
#1046=PLANE('',#8911);
#1047=PLANE('',#8912);
#1048=PLANE('',#8913);
#1049=PLANE('',#8914);
#1050=PLANE('',#8915);
#1051=PLANE('',#8916);
#1052=PLANE('',#8917);
#1053=PLANE('',#8918);
#1054=PLANE('',#8919);
#1055=PLANE('',#8921);
#1056=PLANE('',#8929);
#1057=PLANE('',#8995);
#1058=PLANE('',#8999);
#1059=PLANE('',#9003);
#1060=PLANE('',#9004);
#1061=PLANE('',#9012);
#1062=PLANE('',#9013);
#1063=PLANE('',#9021);
#1064=PLANE('',#9022);
#1065=PLANE('',#9024);
#1066=PLANE('',#9029);
#1067=PLANE('',#9036);
#1068=PLANE('',#9037);
#1069=PLANE('',#9039);
#1070=PLANE('',#9044);
#1071=PLANE('',#9051);
#1072=PLANE('',#9052);
#1073=PLANE('',#9060);
#1074=PLANE('',#9061);
#1075=PLANE('',#9069);
#1076=PLANE('',#9070);
#1077=PLANE('',#9072);
#1078=PLANE('',#9077);
#1079=PLANE('',#9084);
#1080=PLANE('',#9085);
#1081=PLANE('',#9087);
#1082=PLANE('',#9092);
#1083=PLANE('',#9099);
#1084=PLANE('',#9100);
#1085=PLANE('',#9102);
#1086=PLANE('',#9107);
#1087=PLANE('',#9120);
#1088=PLANE('',#9130);
#1089=PLANE('',#9131);
#1090=PLANE('',#9133);
#1091=PLANE('',#9134);
#1092=PLANE('',#9135);
#1093=PLANE('',#9136);
#1094=PLANE('',#9137);
#1095=PLANE('',#9138);
#1096=PLANE('',#9139);
#1097=PLANE('',#9140);
#1098=PLANE('',#9148);
#1099=FACE_OUTER_BOUND('',#1544,.T.);
#1100=FACE_OUTER_BOUND('',#1545,.T.);
#1101=FACE_OUTER_BOUND('',#1546,.T.);
#1102=FACE_OUTER_BOUND('',#1547,.T.);
#1103=FACE_OUTER_BOUND('',#1548,.T.);
#1104=FACE_OUTER_BOUND('',#1549,.T.);
#1105=FACE_OUTER_BOUND('',#1550,.T.);
#1106=FACE_OUTER_BOUND('',#1551,.T.);
#1107=FACE_OUTER_BOUND('',#1552,.T.);
#1108=FACE_OUTER_BOUND('',#1553,.T.);
#1109=FACE_OUTER_BOUND('',#1554,.T.);
#1110=FACE_OUTER_BOUND('',#1555,.T.);
#1111=FACE_OUTER_BOUND('',#1556,.T.);
#1112=FACE_OUTER_BOUND('',#1557,.T.);
#1113=FACE_OUTER_BOUND('',#1558,.T.);
#1114=FACE_OUTER_BOUND('',#1559,.T.);
#1115=FACE_OUTER_BOUND('',#1560,.T.);
#1116=FACE_OUTER_BOUND('',#1573,.T.);
#1117=FACE_OUTER_BOUND('',#1586,.T.);
#1118=FACE_OUTER_BOUND('',#1587,.T.);
#1119=FACE_OUTER_BOUND('',#1588,.T.);
#1120=FACE_OUTER_BOUND('',#1589,.T.);
#1121=FACE_OUTER_BOUND('',#1590,.T.);
#1122=FACE_OUTER_BOUND('',#1591,.T.);
#1123=FACE_OUTER_BOUND('',#1592,.T.);
#1124=FACE_OUTER_BOUND('',#1594,.T.);
#1125=FACE_OUTER_BOUND('',#1595,.T.);
#1126=FACE_OUTER_BOUND('',#1596,.T.);
#1127=FACE_OUTER_BOUND('',#1598,.T.);
#1128=FACE_OUTER_BOUND('',#1599,.T.);
#1129=FACE_OUTER_BOUND('',#1600,.T.);
#1130=FACE_OUTER_BOUND('',#1602,.T.);
#1131=FACE_OUTER_BOUND('',#1604,.T.);
#1132=FACE_OUTER_BOUND('',#1605,.T.);
#1133=FACE_OUTER_BOUND('',#1608,.T.);
#1134=FACE_OUTER_BOUND('',#1609,.T.);
#1135=FACE_OUTER_BOUND('',#1615,.T.);
#1136=FACE_OUTER_BOUND('',#1616,.T.);
#1137=FACE_OUTER_BOUND('',#1617,.T.);
#1138=FACE_OUTER_BOUND('',#1623,.T.);
#1139=FACE_OUTER_BOUND('',#1624,.T.);
#1140=FACE_OUTER_BOUND('',#1625,.T.);
#1141=FACE_OUTER_BOUND('',#1626,.T.);
#1142=FACE_OUTER_BOUND('',#1627,.T.);
#1143=FACE_OUTER_BOUND('',#1628,.T.);
#1144=FACE_OUTER_BOUND('',#1630,.T.);
#1145=FACE_OUTER_BOUND('',#1631,.T.);
#1146=FACE_OUTER_BOUND('',#1632,.T.);
#1147=FACE_OUTER_BOUND('',#1638,.T.);
#1148=FACE_OUTER_BOUND('',#1644,.T.);
#1149=FACE_OUTER_BOUND('',#1645,.T.);
#1150=FACE_OUTER_BOUND('',#1646,.T.);
#1151=FACE_OUTER_BOUND('',#1647,.T.);
#1152=FACE_OUTER_BOUND('',#1648,.T.);
#1153=FACE_OUTER_BOUND('',#1649,.T.);
#1154=FACE_OUTER_BOUND('',#1651,.T.);
#1155=FACE_OUTER_BOUND('',#1652,.T.);
#1156=FACE_OUTER_BOUND('',#1653,.T.);
#1157=FACE_OUTER_BOUND('',#1659,.T.);
#1158=FACE_OUTER_BOUND('',#1665,.T.);
#1159=FACE_OUTER_BOUND('',#1666,.T.);
#1160=FACE_OUTER_BOUND('',#1667,.T.);
#1161=FACE_OUTER_BOUND('',#1668,.T.);
#1162=FACE_OUTER_BOUND('',#1669,.T.);
#1163=FACE_OUTER_BOUND('',#1670,.T.);
#1164=FACE_OUTER_BOUND('',#1671,.T.);
#1165=FACE_OUTER_BOUND('',#1673,.T.);
#1166=FACE_OUTER_BOUND('',#1674,.T.);
#1167=FACE_OUTER_BOUND('',#1675,.T.);
#1168=FACE_OUTER_BOUND('',#1677,.T.);
#1169=FACE_OUTER_BOUND('',#1678,.T.);
#1170=FACE_OUTER_BOUND('',#1679,.T.);
#1171=FACE_OUTER_BOUND('',#1681,.T.);
#1172=FACE_OUTER_BOUND('',#1683,.T.);
#1173=FACE_OUTER_BOUND('',#1684,.T.);
#1174=FACE_OUTER_BOUND('',#1687,.T.);
#1175=FACE_OUTER_BOUND('',#1688,.T.);
#1176=FACE_OUTER_BOUND('',#1694,.T.);
#1177=FACE_OUTER_BOUND('',#1695,.T.);
#1178=FACE_OUTER_BOUND('',#1696,.T.);
#1179=FACE_OUTER_BOUND('',#1702,.T.);
#1180=FACE_OUTER_BOUND('',#1703,.T.);
#1181=FACE_OUTER_BOUND('',#1704,.T.);
#1182=FACE_OUTER_BOUND('',#1705,.T.);
#1183=FACE_OUTER_BOUND('',#1706,.T.);
#1184=FACE_OUTER_BOUND('',#1707,.T.);
#1185=FACE_OUTER_BOUND('',#1709,.T.);
#1186=FACE_OUTER_BOUND('',#1710,.T.);
#1187=FACE_OUTER_BOUND('',#1711,.T.);
#1188=FACE_OUTER_BOUND('',#1717,.T.);
#1189=FACE_OUTER_BOUND('',#1723,.T.);
#1190=FACE_OUTER_BOUND('',#1724,.T.);
#1191=FACE_OUTER_BOUND('',#1725,.T.);
#1192=FACE_OUTER_BOUND('',#1726,.T.);
#1193=FACE_OUTER_BOUND('',#1727,.T.);
#1194=FACE_OUTER_BOUND('',#1728,.T.);
#1195=FACE_OUTER_BOUND('',#1730,.T.);
#1196=FACE_OUTER_BOUND('',#1731,.T.);
#1197=FACE_OUTER_BOUND('',#1732,.T.);
#1198=FACE_OUTER_BOUND('',#1738,.T.);
#1199=FACE_OUTER_BOUND('',#1744,.T.);
#1200=FACE_OUTER_BOUND('',#1745,.T.);
#1201=FACE_OUTER_BOUND('',#1746,.T.);
#1202=FACE_OUTER_BOUND('',#1747,.T.);
#1203=FACE_OUTER_BOUND('',#1748,.T.);
#1204=FACE_OUTER_BOUND('',#1749,.T.);
#1205=FACE_OUTER_BOUND('',#1750,.T.);
#1206=FACE_OUTER_BOUND('',#1751,.T.);
#1207=FACE_OUTER_BOUND('',#1752,.T.);
#1208=FACE_OUTER_BOUND('',#1753,.T.);
#1209=FACE_OUTER_BOUND('',#1754,.T.);
#1210=FACE_OUTER_BOUND('',#1756,.T.);
#1211=FACE_OUTER_BOUND('',#1762,.T.);
#1212=FACE_OUTER_BOUND('',#1768,.T.);
#1213=FACE_OUTER_BOUND('',#1769,.T.);
#1214=FACE_OUTER_BOUND('',#1770,.T.);
#1215=FACE_OUTER_BOUND('',#1771,.T.);
#1216=FACE_OUTER_BOUND('',#1772,.T.);
#1217=FACE_OUTER_BOUND('',#1773,.T.);
#1218=FACE_OUTER_BOUND('',#1775,.T.);
#1219=FACE_OUTER_BOUND('',#1776,.T.);
#1220=FACE_OUTER_BOUND('',#1777,.T.);
#1221=FACE_OUTER_BOUND('',#1783,.T.);
#1222=FACE_OUTER_BOUND('',#1789,.T.);
#1223=FACE_OUTER_BOUND('',#1790,.T.);
#1224=FACE_OUTER_BOUND('',#1791,.T.);
#1225=FACE_OUTER_BOUND('',#1792,.T.);
#1226=FACE_OUTER_BOUND('',#1793,.T.);
#1227=FACE_OUTER_BOUND('',#1794,.T.);
#1228=FACE_OUTER_BOUND('',#1796,.T.);
#1229=FACE_OUTER_BOUND('',#1797,.T.);
#1230=FACE_OUTER_BOUND('',#1798,.T.);
#1231=FACE_OUTER_BOUND('',#1804,.T.);
#1232=FACE_OUTER_BOUND('',#1810,.T.);
#1233=FACE_OUTER_BOUND('',#1811,.T.);
#1234=FACE_OUTER_BOUND('',#1812,.T.);
#1235=FACE_OUTER_BOUND('',#1813,.T.);
#1236=FACE_OUTER_BOUND('',#1814,.T.);
#1237=FACE_OUTER_BOUND('',#1815,.T.);
#1238=FACE_OUTER_BOUND('',#1817,.T.);
#1239=FACE_OUTER_BOUND('',#1818,.T.);
#1240=FACE_OUTER_BOUND('',#1820,.T.);
#1241=FACE_OUTER_BOUND('',#1821,.T.);
#1242=FACE_OUTER_BOUND('',#1823,.T.);
#1243=FACE_OUTER_BOUND('',#1824,.T.);
#1244=FACE_OUTER_BOUND('',#1826,.T.);
#1245=FACE_OUTER_BOUND('',#1827,.T.);
#1246=FACE_OUTER_BOUND('',#1828,.T.);
#1247=FACE_OUTER_BOUND('',#1829,.T.);
#1248=FACE_OUTER_BOUND('',#1830,.T.);
#1249=FACE_OUTER_BOUND('',#1831,.T.);
#1250=FACE_OUTER_BOUND('',#1832,.T.);
#1251=FACE_OUTER_BOUND('',#1833,.T.);
#1252=FACE_OUTER_BOUND('',#1834,.T.);
#1253=FACE_OUTER_BOUND('',#1841,.T.);
#1254=FACE_OUTER_BOUND('',#1846,.T.);
#1255=FACE_OUTER_BOUND('',#1847,.T.);
#1256=FACE_OUTER_BOUND('',#1848,.T.);
#1257=FACE_OUTER_BOUND('',#1850,.T.);
#1258=FACE_OUTER_BOUND('',#1851,.T.);
#1259=FACE_OUTER_BOUND('',#1852,.T.);
#1260=FACE_OUTER_BOUND('',#1854,.T.);
#1261=FACE_OUTER_BOUND('',#1855,.T.);
#1262=FACE_OUTER_BOUND('',#1856,.T.);
#1263=FACE_OUTER_BOUND('',#1857,.T.);
#1264=FACE_OUTER_BOUND('',#1858,.T.);
#1265=FACE_OUTER_BOUND('',#1859,.T.);
#1266=FACE_OUTER_BOUND('',#1862,.T.);
#1267=FACE_OUTER_BOUND('',#1863,.T.);
#1268=FACE_OUTER_BOUND('',#1865,.T.);
#1269=FACE_OUTER_BOUND('',#1866,.T.);
#1270=FACE_OUTER_BOUND('',#1868,.T.);
#1271=FACE_OUTER_BOUND('',#1869,.T.);
#1272=FACE_OUTER_BOUND('',#1870,.T.);
#1273=FACE_OUTER_BOUND('',#1871,.T.);
#1274=FACE_OUTER_BOUND('',#1872,.T.);
#1275=FACE_OUTER_BOUND('',#1874,.T.);
#1276=FACE_OUTER_BOUND('',#1875,.T.);
#1277=FACE_OUTER_BOUND('',#1877,.T.);
#1278=FACE_OUTER_BOUND('',#1878,.T.);
#1279=FACE_OUTER_BOUND('',#1879,.T.);
#1280=FACE_OUTER_BOUND('',#1880,.T.);
#1281=FACE_OUTER_BOUND('',#1881,.T.);
#1282=FACE_OUTER_BOUND('',#1883,.T.);
#1283=FACE_OUTER_BOUND('',#1884,.T.);
#1284=FACE_OUTER_BOUND('',#1886,.T.);
#1285=FACE_OUTER_BOUND('',#1887,.T.);
#1286=FACE_OUTER_BOUND('',#1888,.T.);
#1287=FACE_OUTER_BOUND('',#1889,.T.);
#1288=FACE_OUTER_BOUND('',#1890,.T.);
#1289=FACE_OUTER_BOUND('',#1892,.T.);
#1290=FACE_OUTER_BOUND('',#1893,.T.);
#1291=FACE_OUTER_BOUND('',#1895,.T.);
#1292=FACE_OUTER_BOUND('',#1896,.T.);
#1293=FACE_OUTER_BOUND('',#1897,.T.);
#1294=FACE_OUTER_BOUND('',#1898,.T.);
#1295=FACE_OUTER_BOUND('',#1899,.T.);
#1296=FACE_OUTER_BOUND('',#1900,.T.);
#1297=FACE_OUTER_BOUND('',#1901,.T.);
#1298=FACE_OUTER_BOUND('',#1902,.T.);
#1299=FACE_OUTER_BOUND('',#1903,.T.);
#1300=FACE_OUTER_BOUND('',#1905,.T.);
#1301=FACE_OUTER_BOUND('',#1906,.T.);
#1302=FACE_OUTER_BOUND('',#1908,.T.);
#1303=FACE_OUTER_BOUND('',#1910,.T.);
#1304=FACE_OUTER_BOUND('',#1912,.T.);
#1305=FACE_OUTER_BOUND('',#1913,.T.);
#1306=FACE_OUTER_BOUND('',#1915,.T.);
#1307=FACE_OUTER_BOUND('',#1916,.T.);
#1308=FACE_OUTER_BOUND('',#1922,.T.);
#1309=FACE_OUTER_BOUND('',#1923,.T.);
#1310=FACE_OUTER_BOUND('',#1924,.T.);
#1311=FACE_OUTER_BOUND('',#1925,.T.);
#1312=FACE_OUTER_BOUND('',#1926,.T.);
#1313=FACE_OUTER_BOUND('',#1927,.T.);
#1314=FACE_OUTER_BOUND('',#1928,.T.);
#1315=FACE_OUTER_BOUND('',#1929,.T.);
#1316=FACE_OUTER_BOUND('',#1930,.T.);
#1317=FACE_OUTER_BOUND('',#1931,.T.);
#1318=FACE_OUTER_BOUND('',#1932,.T.);
#1319=FACE_OUTER_BOUND('',#1933,.T.);
#1320=FACE_OUTER_BOUND('',#1934,.T.);
#1321=FACE_OUTER_BOUND('',#1935,.T.);
#1322=FACE_OUTER_BOUND('',#1936,.T.);
#1323=FACE_OUTER_BOUND('',#1937,.T.);
#1324=FACE_OUTER_BOUND('',#1938,.T.);
#1325=FACE_OUTER_BOUND('',#1939,.T.);
#1326=FACE_OUTER_BOUND('',#1940,.T.);
#1327=FACE_OUTER_BOUND('',#1941,.T.);
#1328=FACE_OUTER_BOUND('',#1942,.T.);
#1329=FACE_OUTER_BOUND('',#1943,.T.);
#1330=FACE_OUTER_BOUND('',#1944,.T.);
#1331=FACE_OUTER_BOUND('',#1945,.T.);
#1332=FACE_OUTER_BOUND('',#1946,.T.);
#1333=FACE_OUTER_BOUND('',#1947,.T.);
#1334=FACE_OUTER_BOUND('',#1949,.T.);
#1335=FACE_OUTER_BOUND('',#1950,.T.);
#1336=FACE_OUTER_BOUND('',#1951,.T.);
#1337=FACE_OUTER_BOUND('',#1952,.T.);
#1338=FACE_OUTER_BOUND('',#1953,.T.);
#1339=FACE_OUTER_BOUND('',#1954,.T.);
#1340=FACE_OUTER_BOUND('',#1955,.T.);
#1341=FACE_OUTER_BOUND('',#1957,.T.);
#1342=FACE_OUTER_BOUND('',#1958,.T.);
#1343=FACE_OUTER_BOUND('',#1960,.T.);
#1344=FACE_OUTER_BOUND('',#1961,.T.);
#1345=FACE_OUTER_BOUND('',#1962,.T.);
#1346=FACE_OUTER_BOUND('',#1963,.T.);
#1347=FACE_OUTER_BOUND('',#1965,.T.);
#1348=FACE_OUTER_BOUND('',#1966,.T.);
#1349=FACE_OUTER_BOUND('',#1967,.T.);
#1350=FACE_OUTER_BOUND('',#1968,.T.);
#1351=FACE_OUTER_BOUND('',#1970,.T.);
#1352=FACE_OUTER_BOUND('',#1971,.T.);
#1353=FACE_OUTER_BOUND('',#1972,.T.);
#1354=FACE_OUTER_BOUND('',#1973,.T.);
#1355=FACE_OUTER_BOUND('',#1974,.T.);
#1356=FACE_OUTER_BOUND('',#1975,.T.);
#1357=FACE_OUTER_BOUND('',#1976,.T.);
#1358=FACE_OUTER_BOUND('',#1977,.T.);
#1359=FACE_OUTER_BOUND('',#1978,.T.);
#1360=FACE_OUTER_BOUND('',#1979,.T.);
#1361=FACE_OUTER_BOUND('',#1980,.T.);
#1362=FACE_OUTER_BOUND('',#1981,.T.);
#1363=FACE_OUTER_BOUND('',#1982,.T.);
#1364=FACE_OUTER_BOUND('',#1983,.T.);
#1365=FACE_OUTER_BOUND('',#1984,.T.);
#1366=FACE_OUTER_BOUND('',#1985,.T.);
#1367=FACE_OUTER_BOUND('',#1986,.T.);
#1368=FACE_OUTER_BOUND('',#1987,.T.);
#1369=FACE_OUTER_BOUND('',#1988,.T.);
#1370=FACE_OUTER_BOUND('',#1989,.T.);
#1371=FACE_OUTER_BOUND('',#1990,.T.);
#1372=FACE_OUTER_BOUND('',#1991,.T.);
#1373=FACE_OUTER_BOUND('',#1992,.T.);
#1374=FACE_OUTER_BOUND('',#1993,.T.);
#1375=FACE_OUTER_BOUND('',#1995,.T.);
#1376=FACE_OUTER_BOUND('',#1996,.T.);
#1377=FACE_OUTER_BOUND('',#1998,.T.);
#1378=FACE_OUTER_BOUND('',#1999,.T.);
#1379=FACE_OUTER_BOUND('',#2001,.T.);
#1380=FACE_OUTER_BOUND('',#2002,.T.);
#1381=FACE_OUTER_BOUND('',#2004,.T.);
#1382=FACE_OUTER_BOUND('',#2005,.T.);
#1383=FACE_OUTER_BOUND('',#2007,.T.);
#1384=FACE_OUTER_BOUND('',#2008,.T.);
#1385=FACE_OUTER_BOUND('',#2009,.T.);
#1386=FACE_OUTER_BOUND('',#2010,.T.);
#1387=FACE_OUTER_BOUND('',#2011,.T.);
#1388=FACE_OUTER_BOUND('',#2012,.T.);
#1389=FACE_OUTER_BOUND('',#2014,.T.);
#1390=FACE_OUTER_BOUND('',#2015,.T.);
#1391=FACE_OUTER_BOUND('',#2017,.T.);
#1392=FACE_OUTER_BOUND('',#2018,.T.);
#1393=FACE_OUTER_BOUND('',#2019,.T.);
#1394=FACE_OUTER_BOUND('',#2020,.T.);
#1395=FACE_OUTER_BOUND('',#2022,.T.);
#1396=FACE_OUTER_BOUND('',#2023,.T.);
#1397=FACE_OUTER_BOUND('',#2024,.T.);
#1398=FACE_OUTER_BOUND('',#2025,.T.);
#1399=FACE_OUTER_BOUND('',#2027,.T.);
#1400=FACE_OUTER_BOUND('',#2028,.T.);
#1401=FACE_OUTER_BOUND('',#2029,.T.);
#1402=FACE_OUTER_BOUND('',#2030,.T.);
#1403=FACE_OUTER_BOUND('',#2031,.T.);
#1404=FACE_OUTER_BOUND('',#2032,.T.);
#1405=FACE_OUTER_BOUND('',#2033,.T.);
#1406=FACE_OUTER_BOUND('',#2034,.T.);
#1407=FACE_OUTER_BOUND('',#2035,.T.);
#1408=FACE_OUTER_BOUND('',#2036,.T.);
#1409=FACE_OUTER_BOUND('',#2037,.T.);
#1410=FACE_OUTER_BOUND('',#2038,.T.);
#1411=FACE_OUTER_BOUND('',#2039,.T.);
#1412=FACE_OUTER_BOUND('',#2040,.T.);
#1413=FACE_OUTER_BOUND('',#2041,.T.);
#1414=FACE_OUTER_BOUND('',#2042,.T.);
#1415=FACE_OUTER_BOUND('',#2043,.T.);
#1416=FACE_OUTER_BOUND('',#2044,.T.);
#1417=FACE_OUTER_BOUND('',#2045,.T.);
#1418=FACE_OUTER_BOUND('',#2046,.T.);
#1419=FACE_OUTER_BOUND('',#2047,.T.);
#1420=FACE_OUTER_BOUND('',#2048,.T.);
#1421=FACE_OUTER_BOUND('',#2049,.T.);
#1422=FACE_OUTER_BOUND('',#2050,.T.);
#1423=FACE_OUTER_BOUND('',#2051,.T.);
#1424=FACE_OUTER_BOUND('',#2052,.T.);
#1425=FACE_OUTER_BOUND('',#2053,.T.);
#1426=FACE_OUTER_BOUND('',#2055,.T.);
#1427=FACE_OUTER_BOUND('',#2056,.T.);
#1428=FACE_OUTER_BOUND('',#2058,.T.);
#1429=FACE_OUTER_BOUND('',#2059,.T.);
#1430=FACE_OUTER_BOUND('',#2061,.T.);
#1431=FACE_OUTER_BOUND('',#2062,.T.);
#1432=FACE_OUTER_BOUND('',#2064,.T.);
#1433=FACE_OUTER_BOUND('',#2065,.T.);
#1434=FACE_OUTER_BOUND('',#2067,.T.);
#1435=FACE_OUTER_BOUND('',#2068,.T.);
#1436=FACE_OUTER_BOUND('',#2069,.T.);
#1437=FACE_OUTER_BOUND('',#2070,.T.);
#1438=FACE_OUTER_BOUND('',#2071,.T.);
#1439=FACE_OUTER_BOUND('',#2072,.T.);
#1440=FACE_OUTER_BOUND('',#2074,.T.);
#1441=FACE_OUTER_BOUND('',#2075,.T.);
#1442=FACE_OUTER_BOUND('',#2076,.T.);
#1443=FACE_OUTER_BOUND('',#2077,.T.);
#1444=FACE_OUTER_BOUND('',#2078,.T.);
#1445=FACE_OUTER_BOUND('',#2079,.T.);
#1446=FACE_OUTER_BOUND('',#2080,.T.);
#1447=FACE_OUTER_BOUND('',#2081,.T.);
#1448=FACE_OUTER_BOUND('',#2082,.T.);
#1449=FACE_OUTER_BOUND('',#2083,.T.);
#1450=FACE_OUTER_BOUND('',#2084,.T.);
#1451=FACE_OUTER_BOUND('',#2085,.T.);
#1452=FACE_OUTER_BOUND('',#2086,.T.);
#1453=FACE_OUTER_BOUND('',#2087,.T.);
#1454=FACE_OUTER_BOUND('',#2088,.T.);
#1455=FACE_OUTER_BOUND('',#2089,.T.);
#1456=FACE_OUTER_BOUND('',#2090,.T.);
#1457=FACE_OUTER_BOUND('',#2091,.T.);
#1458=FACE_OUTER_BOUND('',#2092,.T.);
#1459=FACE_OUTER_BOUND('',#2093,.T.);
#1460=FACE_OUTER_BOUND('',#2094,.T.);
#1461=FACE_OUTER_BOUND('',#2095,.T.);
#1462=FACE_OUTER_BOUND('',#2096,.T.);
#1463=FACE_OUTER_BOUND('',#2097,.T.);
#1464=FACE_OUTER_BOUND('',#2098,.T.);
#1465=FACE_OUTER_BOUND('',#2099,.T.);
#1466=FACE_OUTER_BOUND('',#2101,.T.);
#1467=FACE_OUTER_BOUND('',#2102,.T.);
#1468=FACE_OUTER_BOUND('',#2103,.T.);
#1469=FACE_OUTER_BOUND('',#2104,.T.);
#1470=FACE_OUTER_BOUND('',#2105,.T.);
#1471=FACE_OUTER_BOUND('',#2106,.T.);
#1472=FACE_OUTER_BOUND('',#2107,.T.);
#1473=FACE_OUTER_BOUND('',#2108,.T.);
#1474=FACE_OUTER_BOUND('',#2110,.T.);
#1475=FACE_OUTER_BOUND('',#2112,.T.);
#1476=FACE_OUTER_BOUND('',#2113,.T.);
#1477=FACE_OUTER_BOUND('',#2114,.T.);
#1478=FACE_OUTER_BOUND('',#2116,.T.);
#1479=FACE_OUTER_BOUND('',#2118,.T.);
#1480=FACE_OUTER_BOUND('',#2119,.T.);
#1481=FACE_OUTER_BOUND('',#2120,.T.);
#1482=FACE_OUTER_BOUND('',#2122,.T.);
#1483=FACE_OUTER_BOUND('',#2124,.T.);
#1484=FACE_OUTER_BOUND('',#2125,.T.);
#1485=FACE_OUTER_BOUND('',#2126,.T.);
#1486=FACE_OUTER_BOUND('',#2127,.T.);
#1487=FACE_OUTER_BOUND('',#2129,.T.);
#1488=FACE_OUTER_BOUND('',#2131,.T.);
#1489=FACE_OUTER_BOUND('',#2133,.T.);
#1490=FACE_OUTER_BOUND('',#2135,.T.);
#1491=FACE_OUTER_BOUND('',#2136,.T.);
#1492=FACE_OUTER_BOUND('',#2137,.T.);
#1493=FACE_OUTER_BOUND('',#2138,.T.);
#1494=FACE_OUTER_BOUND('',#2140,.T.);
#1495=FACE_OUTER_BOUND('',#2142,.T.);
#1496=FACE_OUTER_BOUND('',#2144,.T.);
#1497=FACE_OUTER_BOUND('',#2146,.T.);
#1498=FACE_OUTER_BOUND('',#2147,.T.);
#1499=FACE_OUTER_BOUND('',#2148,.T.);
#1500=FACE_OUTER_BOUND('',#2150,.T.);
#1501=FACE_OUTER_BOUND('',#2152,.T.);
#1502=FACE_OUTER_BOUND('',#2153,.T.);
#1503=FACE_OUTER_BOUND('',#2154,.T.);
#1504=FACE_OUTER_BOUND('',#2156,.T.);
#1505=FACE_OUTER_BOUND('',#2158,.T.);
#1506=FACE_OUTER_BOUND('',#2159,.T.);
#1507=FACE_OUTER_BOUND('',#2160,.T.);
#1508=FACE_OUTER_BOUND('',#2161,.T.);
#1509=FACE_OUTER_BOUND('',#2163,.T.);
#1510=FACE_OUTER_BOUND('',#2165,.T.);
#1511=FACE_OUTER_BOUND('',#2167,.T.);
#1512=FACE_OUTER_BOUND('',#2169,.T.);
#1513=FACE_OUTER_BOUND('',#2170,.T.);
#1514=FACE_OUTER_BOUND('',#2171,.T.);
#1515=FACE_OUTER_BOUND('',#2172,.T.);
#1516=FACE_OUTER_BOUND('',#2174,.T.);
#1517=FACE_OUTER_BOUND('',#2176,.T.);
#1518=FACE_OUTER_BOUND('',#2178,.T.);
#1519=FACE_OUTER_BOUND('',#2180,.T.);
#1520=FACE_OUTER_BOUND('',#2181,.T.);
#1521=FACE_OUTER_BOUND('',#2182,.T.);
#1522=FACE_OUTER_BOUND('',#2183,.T.);
#1523=FACE_OUTER_BOUND('',#2184,.T.);
#1524=FACE_OUTER_BOUND('',#2185,.T.);
#1525=FACE_OUTER_BOUND('',#2186,.T.);
#1526=FACE_OUTER_BOUND('',#2187,.T.);
#1527=FACE_OUTER_BOUND('',#2193,.T.);
#1528=FACE_OUTER_BOUND('',#2194,.T.);
#1529=FACE_OUTER_BOUND('',#2196,.T.);
#1530=FACE_OUTER_BOUND('',#2198,.T.);
#1531=FACE_OUTER_BOUND('',#2200,.T.);
#1532=FACE_OUTER_BOUND('',#2206,.T.);
#1533=FACE_OUTER_BOUND('',#2207,.T.);
#1534=FACE_OUTER_BOUND('',#2208,.T.);
#1535=FACE_OUTER_BOUND('',#2209,.T.);
#1536=FACE_OUTER_BOUND('',#2210,.T.);
#1537=FACE_OUTER_BOUND('',#2211,.T.);
#1538=FACE_OUTER_BOUND('',#2212,.T.);
#1539=FACE_OUTER_BOUND('',#2213,.T.);
#1540=FACE_OUTER_BOUND('',#2215,.T.);
#1541=FACE_OUTER_BOUND('',#2216,.T.);
#1542=FACE_OUTER_BOUND('',#2217,.T.);
#1543=FACE_OUTER_BOUND('',#2218,.T.);
#1544=EDGE_LOOP('',(#5148,#5149,#5150,#5151));
#1545=EDGE_LOOP('',(#5152,#5153,#5154,#5155));
#1546=EDGE_LOOP('',(#5156,#5157,#5158,#5159));
#1547=EDGE_LOOP('',(#5160,#5161,#5162,#5163));
#1548=EDGE_LOOP('',(#5164,#5165,#5166,#5167));
#1549=EDGE_LOOP('',(#5168,#5169,#5170,#5171));
#1550=EDGE_LOOP('',(#5172,#5173,#5174,#5175));
#1551=EDGE_LOOP('',(#5176,#5177,#5178,#5179));
#1552=EDGE_LOOP('',(#5180,#5181,#5182,#5183));
#1553=EDGE_LOOP('',(#5184,#5185,#5186,#5187));
#1554=EDGE_LOOP('',(#5188,#5189,#5190,#5191));
#1555=EDGE_LOOP('',(#5192,#5193,#5194,#5195));
#1556=EDGE_LOOP('',(#5196,#5197,#5198,#5199));
#1557=EDGE_LOOP('',(#5200,#5201,#5202,#5203));
#1558=EDGE_LOOP('',(#5204,#5205,#5206,#5207));
#1559=EDGE_LOOP('',(#5208,#5209,#5210,#5211));
#1560=EDGE_LOOP('',(#5212,#5213,#5214,#5215));
#1561=EDGE_LOOP('',(#5216));
#1562=EDGE_LOOP('',(#5217));
#1563=EDGE_LOOP('',(#5218));
#1564=EDGE_LOOP('',(#5219));
#1565=EDGE_LOOP('',(#5220));
#1566=EDGE_LOOP('',(#5221));
#1567=EDGE_LOOP('',(#5222));
#1568=EDGE_LOOP('',(#5223));
#1569=EDGE_LOOP('',(#5224));
#1570=EDGE_LOOP('',(#5225));
#1571=EDGE_LOOP('',(#5226));
#1572=EDGE_LOOP('',(#5227));
#1573=EDGE_LOOP('',(#5228,#5229,#5230,#5231));
#1574=EDGE_LOOP('',(#5232));
#1575=EDGE_LOOP('',(#5233));
#1576=EDGE_LOOP('',(#5234));
#1577=EDGE_LOOP('',(#5235));
#1578=EDGE_LOOP('',(#5236));
#1579=EDGE_LOOP('',(#5237));
#1580=EDGE_LOOP('',(#5238));
#1581=EDGE_LOOP('',(#5239));
#1582=EDGE_LOOP('',(#5240));
#1583=EDGE_LOOP('',(#5241));
#1584=EDGE_LOOP('',(#5242));
#1585=EDGE_LOOP('',(#5243));
#1586=EDGE_LOOP('',(#5244,#5245,#5246,#5247));
#1587=EDGE_LOOP('',(#5248,#5249,#5250,#5251));
#1588=EDGE_LOOP('',(#5252,#5253,#5254,#5255));
#1589=EDGE_LOOP('',(#5256,#5257,#5258,#5259));
#1590=EDGE_LOOP('',(#5260,#5261));
#1591=EDGE_LOOP('',(#5262,#5263,#5264,#5265,#5266,#5267));
#1592=EDGE_LOOP('',(#5268));
#1593=EDGE_LOOP('',(#5269));
#1594=EDGE_LOOP('',(#5270,#5271,#5272));
#1595=EDGE_LOOP('',(#5273,#5274,#5275,#5276,#5277,#5278));
#1596=EDGE_LOOP('',(#5279));
#1597=EDGE_LOOP('',(#5280));
#1598=EDGE_LOOP('',(#5281,#5282,#5283,#5284));
#1599=EDGE_LOOP('',(#5285,#5286,#5287,#5288));
#1600=EDGE_LOOP('',(#5289,#5290,#5291,#5292));
#1601=EDGE_LOOP('',(#5293,#5294));
#1602=EDGE_LOOP('',(#5295,#5296,#5297,#5298));
#1603=EDGE_LOOP('',(#5299,#5300,#5301));
#1604=EDGE_LOOP('',(#5302,#5303,#5304,#5305));
#1605=EDGE_LOOP('',(#5306,#5307,#5308,#5309));
#1606=EDGE_LOOP('',(#5310));
#1607=EDGE_LOOP('',(#5311));
#1608=EDGE_LOOP('',(#5312,#5313,#5314,#5315));
#1609=EDGE_LOOP('',(#5316,#5317,#5318,#5319,#5320,#5321));
#1610=EDGE_LOOP('',(#5322));
#1611=EDGE_LOOP('',(#5323));
#1612=EDGE_LOOP('',(#5324));
#1613=EDGE_LOOP('',(#5325));
#1614=EDGE_LOOP('',(#5326));
#1615=EDGE_LOOP('',(#5327,#5328,#5329,#5330));
#1616=EDGE_LOOP('',(#5331,#5332,#5333,#5334));
#1617=EDGE_LOOP('',(#5335,#5336,#5337,#5338,#5339,#5340));
#1618=EDGE_LOOP('',(#5341));
#1619=EDGE_LOOP('',(#5342));
#1620=EDGE_LOOP('',(#5343));
#1621=EDGE_LOOP('',(#5344));
#1622=EDGE_LOOP('',(#5345));
#1623=EDGE_LOOP('',(#5346,#5347,#5348,#5349));
#1624=EDGE_LOOP('',(#5350,#5351,#5352,#5353));
#1625=EDGE_LOOP('',(#5354,#5355,#5356,#5357));
#1626=EDGE_LOOP('',(#5358,#5359,#5360,#5361));
#1627=EDGE_LOOP('',(#5362,#5363,#5364,#5365));
#1628=EDGE_LOOP('',(#5366));
#1629=EDGE_LOOP('',(#5367));
#1630=EDGE_LOOP('',(#5368,#5369,#5370,#5371));
#1631=EDGE_LOOP('',(#5372,#5373,#5374,#5375));
#1632=EDGE_LOOP('',(#5376));
#1633=EDGE_LOOP('',(#5377));
#1634=EDGE_LOOP('',(#5378));
#1635=EDGE_LOOP('',(#5379));
#1636=EDGE_LOOP('',(#5380));
#1637=EDGE_LOOP('',(#5381));
#1638=EDGE_LOOP('',(#5382));
#1639=EDGE_LOOP('',(#5383));
#1640=EDGE_LOOP('',(#5384));
#1641=EDGE_LOOP('',(#5385));
#1642=EDGE_LOOP('',(#5386));
#1643=EDGE_LOOP('',(#5387));
#1644=EDGE_LOOP('',(#5388,#5389,#5390,#5391));
#1645=EDGE_LOOP('',(#5392,#5393,#5394,#5395));
#1646=EDGE_LOOP('',(#5396,#5397,#5398,#5399));
#1647=EDGE_LOOP('',(#5400,#5401,#5402,#5403));
#1648=EDGE_LOOP('',(#5404,#5405,#5406,#5407));
#1649=EDGE_LOOP('',(#5408));
#1650=EDGE_LOOP('',(#5409));
#1651=EDGE_LOOP('',(#5410,#5411,#5412,#5413));
#1652=EDGE_LOOP('',(#5414,#5415,#5416,#5417));
#1653=EDGE_LOOP('',(#5418));
#1654=EDGE_LOOP('',(#5419));
#1655=EDGE_LOOP('',(#5420));
#1656=EDGE_LOOP('',(#5421));
#1657=EDGE_LOOP('',(#5422));
#1658=EDGE_LOOP('',(#5423));
#1659=EDGE_LOOP('',(#5424));
#1660=EDGE_LOOP('',(#5425));
#1661=EDGE_LOOP('',(#5426));
#1662=EDGE_LOOP('',(#5427));
#1663=EDGE_LOOP('',(#5428));
#1664=EDGE_LOOP('',(#5429));
#1665=EDGE_LOOP('',(#5430,#5431,#5432,#5433));
#1666=EDGE_LOOP('',(#5434,#5435,#5436,#5437));
#1667=EDGE_LOOP('',(#5438,#5439,#5440,#5441));
#1668=EDGE_LOOP('',(#5442,#5443,#5444,#5445));
#1669=EDGE_LOOP('',(#5446,#5447));
#1670=EDGE_LOOP('',(#5448,#5449,#5450,#5451,#5452,#5453));
#1671=EDGE_LOOP('',(#5454));
#1672=EDGE_LOOP('',(#5455));
#1673=EDGE_LOOP('',(#5456,#5457,#5458));
#1674=EDGE_LOOP('',(#5459,#5460,#5461,#5462,#5463,#5464));
#1675=EDGE_LOOP('',(#5465));
#1676=EDGE_LOOP('',(#5466));
#1677=EDGE_LOOP('',(#5467,#5468,#5469,#5470));
#1678=EDGE_LOOP('',(#5471,#5472,#5473,#5474));
#1679=EDGE_LOOP('',(#5475,#5476,#5477,#5478));
#1680=EDGE_LOOP('',(#5479,#5480));
#1681=EDGE_LOOP('',(#5481,#5482,#5483,#5484));
#1682=EDGE_LOOP('',(#5485,#5486,#5487));
#1683=EDGE_LOOP('',(#5488,#5489,#5490,#5491));
#1684=EDGE_LOOP('',(#5492,#5493,#5494,#5495));
#1685=EDGE_LOOP('',(#5496));
#1686=EDGE_LOOP('',(#5497));
#1687=EDGE_LOOP('',(#5498,#5499,#5500,#5501));
#1688=EDGE_LOOP('',(#5502,#5503,#5504,#5505,#5506,#5507));
#1689=EDGE_LOOP('',(#5508));
#1690=EDGE_LOOP('',(#5509));
#1691=EDGE_LOOP('',(#5510));
#1692=EDGE_LOOP('',(#5511));
#1693=EDGE_LOOP('',(#5512));
#1694=EDGE_LOOP('',(#5513,#5514,#5515,#5516));
#1695=EDGE_LOOP('',(#5517,#5518,#5519,#5520));
#1696=EDGE_LOOP('',(#5521,#5522,#5523,#5524,#5525,#5526));
#1697=EDGE_LOOP('',(#5527));
#1698=EDGE_LOOP('',(#5528));
#1699=EDGE_LOOP('',(#5529));
#1700=EDGE_LOOP('',(#5530));
#1701=EDGE_LOOP('',(#5531));
#1702=EDGE_LOOP('',(#5532,#5533,#5534,#5535));
#1703=EDGE_LOOP('',(#5536,#5537,#5538,#5539));
#1704=EDGE_LOOP('',(#5540,#5541,#5542,#5543));
#1705=EDGE_LOOP('',(#5544,#5545,#5546,#5547));
#1706=EDGE_LOOP('',(#5548,#5549,#5550,#5551));
#1707=EDGE_LOOP('',(#5552));
#1708=EDGE_LOOP('',(#5553));
#1709=EDGE_LOOP('',(#5554,#5555,#5556,#5557));
#1710=EDGE_LOOP('',(#5558,#5559,#5560,#5561));
#1711=EDGE_LOOP('',(#5562));
#1712=EDGE_LOOP('',(#5563));
#1713=EDGE_LOOP('',(#5564));
#1714=EDGE_LOOP('',(#5565));
#1715=EDGE_LOOP('',(#5566));
#1716=EDGE_LOOP('',(#5567));
#1717=EDGE_LOOP('',(#5568));
#1718=EDGE_LOOP('',(#5569));
#1719=EDGE_LOOP('',(#5570));
#1720=EDGE_LOOP('',(#5571));
#1721=EDGE_LOOP('',(#5572));
#1722=EDGE_LOOP('',(#5573));
#1723=EDGE_LOOP('',(#5574,#5575,#5576,#5577));
#1724=EDGE_LOOP('',(#5578,#5579,#5580,#5581));
#1725=EDGE_LOOP('',(#5582,#5583,#5584,#5585));
#1726=EDGE_LOOP('',(#5586,#5587,#5588,#5589));
#1727=EDGE_LOOP('',(#5590,#5591,#5592,#5593));
#1728=EDGE_LOOP('',(#5594));
#1729=EDGE_LOOP('',(#5595));
#1730=EDGE_LOOP('',(#5596,#5597,#5598,#5599));
#1731=EDGE_LOOP('',(#5600,#5601,#5602,#5603));
#1732=EDGE_LOOP('',(#5604));
#1733=EDGE_LOOP('',(#5605));
#1734=EDGE_LOOP('',(#5606));
#1735=EDGE_LOOP('',(#5607));
#1736=EDGE_LOOP('',(#5608));
#1737=EDGE_LOOP('',(#5609));
#1738=EDGE_LOOP('',(#5610));
#1739=EDGE_LOOP('',(#5611));
#1740=EDGE_LOOP('',(#5612));
#1741=EDGE_LOOP('',(#5613));
#1742=EDGE_LOOP('',(#5614));
#1743=EDGE_LOOP('',(#5615));
#1744=EDGE_LOOP('',(#5616,#5617,#5618,#5619));
#1745=EDGE_LOOP('',(#5620,#5621,#5622,#5623));
#1746=EDGE_LOOP('',(#5624,#5625,#5626,#5627));
#1747=EDGE_LOOP('',(#5628,#5629,#5630,#5631));
#1748=EDGE_LOOP('',(#5632,#5633,#5634,#5635));
#1749=EDGE_LOOP('',(#5636,#5637,#5638,#5639));
#1750=EDGE_LOOP('',(#5640,#5641,#5642,#5643));
#1751=EDGE_LOOP('',(#5644,#5645,#5646,#5647));
#1752=EDGE_LOOP('',(#5648,#5649,#5650,#5651));
#1753=EDGE_LOOP('',(#5652,#5653,#5654,#5655));
#1754=EDGE_LOOP('',(#5656,#5657,#5658,#5659));
#1755=EDGE_LOOP('',(#5660,#5661,#5662,#5663));
#1756=EDGE_LOOP('',(#5664));
#1757=EDGE_LOOP('',(#5665));
#1758=EDGE_LOOP('',(#5666));
#1759=EDGE_LOOP('',(#5667));
#1760=EDGE_LOOP('',(#5668));
#1761=EDGE_LOOP('',(#5669));
#1762=EDGE_LOOP('',(#5670));
#1763=EDGE_LOOP('',(#5671));
#1764=EDGE_LOOP('',(#5672));
#1765=EDGE_LOOP('',(#5673));
#1766=EDGE_LOOP('',(#5674));
#1767=EDGE_LOOP('',(#5675));
#1768=EDGE_LOOP('',(#5676,#5677,#5678,#5679));
#1769=EDGE_LOOP('',(#5680,#5681,#5682,#5683));
#1770=EDGE_LOOP('',(#5684,#5685,#5686,#5687));
#1771=EDGE_LOOP('',(#5688,#5689,#5690,#5691));
#1772=EDGE_LOOP('',(#5692,#5693,#5694,#5695));
#1773=EDGE_LOOP('',(#5696));
#1774=EDGE_LOOP('',(#5697));
#1775=EDGE_LOOP('',(#5698,#5699,#5700,#5701));
#1776=EDGE_LOOP('',(#5702,#5703,#5704,#5705));
#1777=EDGE_LOOP('',(#5706));
#1778=EDGE_LOOP('',(#5707));
#1779=EDGE_LOOP('',(#5708));
#1780=EDGE_LOOP('',(#5709));
#1781=EDGE_LOOP('',(#5710));
#1782=EDGE_LOOP('',(#5711));
#1783=EDGE_LOOP('',(#5712));
#1784=EDGE_LOOP('',(#5713));
#1785=EDGE_LOOP('',(#5714));
#1786=EDGE_LOOP('',(#5715));
#1787=EDGE_LOOP('',(#5716));
#1788=EDGE_LOOP('',(#5717));
#1789=EDGE_LOOP('',(#5718,#5719,#5720,#5721));
#1790=EDGE_LOOP('',(#5722,#5723,#5724,#5725));
#1791=EDGE_LOOP('',(#5726,#5727,#5728,#5729));
#1792=EDGE_LOOP('',(#5730,#5731,#5732,#5733));
#1793=EDGE_LOOP('',(#5734,#5735,#5736,#5737));
#1794=EDGE_LOOP('',(#5738));
#1795=EDGE_LOOP('',(#5739));
#1796=EDGE_LOOP('',(#5740,#5741,#5742,#5743));
#1797=EDGE_LOOP('',(#5744,#5745,#5746,#5747));
#1798=EDGE_LOOP('',(#5748));
#1799=EDGE_LOOP('',(#5749));
#1800=EDGE_LOOP('',(#5750));
#1801=EDGE_LOOP('',(#5751));
#1802=EDGE_LOOP('',(#5752));
#1803=EDGE_LOOP('',(#5753));
#1804=EDGE_LOOP('',(#5754));
#1805=EDGE_LOOP('',(#5755));
#1806=EDGE_LOOP('',(#5756));
#1807=EDGE_LOOP('',(#5757));
#1808=EDGE_LOOP('',(#5758));
#1809=EDGE_LOOP('',(#5759));
#1810=EDGE_LOOP('',(#5760,#5761,#5762,#5763));
#1811=EDGE_LOOP('',(#5764));
#1812=EDGE_LOOP('',(#5765,#5766,#5767,#5768));
#1813=EDGE_LOOP('',(#5769));
#1814=EDGE_LOOP('',(#5770,#5771,#5772,#5773));
#1815=EDGE_LOOP('',(#5774));
#1816=EDGE_LOOP('',(#5775));
#1817=EDGE_LOOP('',(#5776,#5777,#5778,#5779));
#1818=EDGE_LOOP('',(#5780));
#1819=EDGE_LOOP('',(#5781));
#1820=EDGE_LOOP('',(#5782,#5783,#5784,#5785));
#1821=EDGE_LOOP('',(#5786));
#1822=EDGE_LOOP('',(#5787));
#1823=EDGE_LOOP('',(#5788,#5789,#5790,#5791));
#1824=EDGE_LOOP('',(#5792));
#1825=EDGE_LOOP('',(#5793));
#1826=EDGE_LOOP('',(#5794,#5795,#5796,#5797));
#1827=EDGE_LOOP('',(#5798,#5799,#5800,#5801));
#1828=EDGE_LOOP('',(#5802,#5803,#5804,#5805));
#1829=EDGE_LOOP('',(#5806,#5807,#5808,#5809));
#1830=EDGE_LOOP('',(#5810,#5811,#5812,#5813));
#1831=EDGE_LOOP('',(#5814,#5815,#5816,#5817));
#1832=EDGE_LOOP('',(#5818,#5819,#5820,#5821));
#1833=EDGE_LOOP('',(#5822,#5823,#5824,#5825));
#1834=EDGE_LOOP('',(#5826,#5827,#5828,#5829));
#1835=EDGE_LOOP('',(#5830));
#1836=EDGE_LOOP('',(#5831));
#1837=EDGE_LOOP('',(#5832));
#1838=EDGE_LOOP('',(#5833));
#1839=EDGE_LOOP('',(#5834));
#1840=EDGE_LOOP('',(#5835));
#1841=EDGE_LOOP('',(#5836,#5837,#5838,#5839));
#1842=EDGE_LOOP('',(#5840));
#1843=EDGE_LOOP('',(#5841));
#1844=EDGE_LOOP('',(#5842));
#1845=EDGE_LOOP('',(#5843));
#1846=EDGE_LOOP('',(#5844,#5845,#5846,#5847));
#1847=EDGE_LOOP('',(#5848,#5849,#5850,#5851));
#1848=EDGE_LOOP('',(#5852,#5853,#5854,#5855));
#1849=EDGE_LOOP('',(#5856));
#1850=EDGE_LOOP('',(#5857,#5858,#5859,#5860));
#1851=EDGE_LOOP('',(#5861,#5862,#5863,#5864));
#1852=EDGE_LOOP('',(#5865,#5866,#5867,#5868));
#1853=EDGE_LOOP('',(#5869));
#1854=EDGE_LOOP('',(#5870,#5871,#5872,#5873));
#1855=EDGE_LOOP('',(#5874,#5875,#5876,#5877,#5878,#5879,#5880,#5881));
#1856=EDGE_LOOP('',(#5882,#5883,#5884,#5885));
#1857=EDGE_LOOP('',(#5886,#5887,#5888,#5889,#5890,#5891,#5892,#5893));
#1858=EDGE_LOOP('',(#5894,#5895,#5896,#5897));
#1859=EDGE_LOOP('',(#5898,#5899,#5900,#5901));
#1860=EDGE_LOOP('',(#5902));
#1861=EDGE_LOOP('',(#5903));
#1862=EDGE_LOOP('',(#5904,#5905,#5906,#5907));
#1863=EDGE_LOOP('',(#5908));
#1864=EDGE_LOOP('',(#5909));
#1865=EDGE_LOOP('',(#5910,#5911,#5912,#5913));
#1866=EDGE_LOOP('',(#5914));
#1867=EDGE_LOOP('',(#5915,#5916,#5917,#5918));
#1868=EDGE_LOOP('',(#5919,#5920,#5921,#5922));
#1869=EDGE_LOOP('',(#5923,#5924,#5925,#5926,#5927,#5928,#5929,#5930));
#1870=EDGE_LOOP('',(#5931,#5932,#5933,#5934,#5935,#5936,#5937,#5938));
#1871=EDGE_LOOP('',(#5939,#5940,#5941,#5942));
#1872=EDGE_LOOP('',(#5943));
#1873=EDGE_LOOP('',(#5944));
#1874=EDGE_LOOP('',(#5945,#5946,#5947,#5948));
#1875=EDGE_LOOP('',(#5949));
#1876=EDGE_LOOP('',(#5950,#5951,#5952,#5953));
#1877=EDGE_LOOP('',(#5954,#5955,#5956,#5957));
#1878=EDGE_LOOP('',(#5958,#5959,#5960,#5961));
#1879=EDGE_LOOP('',(#5962,#5963,#5964,#5965));
#1880=EDGE_LOOP('',(#5966,#5967,#5968,#5969));
#1881=EDGE_LOOP('',(#5970));
#1882=EDGE_LOOP('',(#5971));
#1883=EDGE_LOOP('',(#5972,#5973,#5974,#5975));
#1884=EDGE_LOOP('',(#5976));
#1885=EDGE_LOOP('',(#5977,#5978,#5979,#5980));
#1886=EDGE_LOOP('',(#5981,#5982,#5983,#5984));
#1887=EDGE_LOOP('',(#5985,#5986,#5987,#5988));
#1888=EDGE_LOOP('',(#5989,#5990,#5991,#5992));
#1889=EDGE_LOOP('',(#5993,#5994,#5995,#5996));
#1890=EDGE_LOOP('',(#5997));
#1891=EDGE_LOOP('',(#5998));
#1892=EDGE_LOOP('',(#5999,#6000,#6001,#6002));
#1893=EDGE_LOOP('',(#6003));
#1894=EDGE_LOOP('',(#6004,#6005,#6006,#6007));
#1895=EDGE_LOOP('',(#6008,#6009,#6010,#6011));
#1896=EDGE_LOOP('',(#6012,#6013,#6014,#6015,#6016,#6017,#6018,#6019));
#1897=EDGE_LOOP('',(#6020,#6021,#6022,#6023));
#1898=EDGE_LOOP('',(#6024,#6025,#6026,#6027));
#1899=EDGE_LOOP('',(#6028,#6029,#6030,#6031));
#1900=EDGE_LOOP('',(#6032,#6033,#6034,#6035));
#1901=EDGE_LOOP('',(#6036,#6037,#6038,#6039));
#1902=EDGE_LOOP('',(#6040,#6041,#6042,#6043));
#1903=EDGE_LOOP('',(#6044));
#1904=EDGE_LOOP('',(#6045));
#1905=EDGE_LOOP('',(#6046,#6047,#6048,#6049));
#1906=EDGE_LOOP('',(#6050,#6051,#6052,#6053,#6054,#6055,#6056,#6057,#6058,
#6059,#6060,#6061));
#1907=EDGE_LOOP('',(#6062,#6063,#6064,#6065));
#1908=EDGE_LOOP('',(#6066));
#1909=EDGE_LOOP('',(#6067));
#1910=EDGE_LOOP('',(#6068));
#1911=EDGE_LOOP('',(#6069));
#1912=EDGE_LOOP('',(#6070,#6071,#6072,#6073));
#1913=EDGE_LOOP('',(#6074));
#1914=EDGE_LOOP('',(#6075));
#1915=EDGE_LOOP('',(#6076,#6077,#6078,#6079,#6080,#6081,#6082,#6083));
#1916=EDGE_LOOP('',(#6084,#6085,#6086,#6087));
#1917=EDGE_LOOP('',(#6088));
#1918=EDGE_LOOP('',(#6089));
#1919=EDGE_LOOP('',(#6090));
#1920=EDGE_LOOP('',(#6091));
#1921=EDGE_LOOP('',(#6092,#6093,#6094,#6095));
#1922=EDGE_LOOP('',(#6096,#6097,#6098,#6099));
#1923=EDGE_LOOP('',(#6100,#6101,#6102,#6103));
#1924=EDGE_LOOP('',(#6104,#6105,#6106,#6107));
#1925=EDGE_LOOP('',(#6108,#6109,#6110,#6111));
#1926=EDGE_LOOP('',(#6112,#6113,#6114,#6115));
#1927=EDGE_LOOP('',(#6116,#6117,#6118,#6119));
#1928=EDGE_LOOP('',(#6120,#6121,#6122,#6123));
#1929=EDGE_LOOP('',(#6124,#6125,#6126,#6127));
#1930=EDGE_LOOP('',(#6128,#6129,#6130,#6131));
#1931=EDGE_LOOP('',(#6132,#6133,#6134,#6135));
#1932=EDGE_LOOP('',(#6136,#6137,#6138,#6139));
#1933=EDGE_LOOP('',(#6140,#6141,#6142,#6143));
#1934=EDGE_LOOP('',(#6144,#6145,#6146,#6147));
#1935=EDGE_LOOP('',(#6148,#6149,#6150,#6151));
#1936=EDGE_LOOP('',(#6152,#6153,#6154,#6155));
#1937=EDGE_LOOP('',(#6156,#6157,#6158,#6159));
#1938=EDGE_LOOP('',(#6160,#6161,#6162,#6163));
#1939=EDGE_LOOP('',(#6164,#6165,#6166,#6167));
#1940=EDGE_LOOP('',(#6168,#6169,#6170,#6171,#6172,#6173));
#1941=EDGE_LOOP('',(#6174,#6175,#6176,#6177,#6178,#6179));
#1942=EDGE_LOOP('',(#6180));
#1943=EDGE_LOOP('',(#6181));
#1944=EDGE_LOOP('',(#6182,#6183,#6184,#6185));
#1945=EDGE_LOOP('',(#6186,#6187,#6188,#6189));
#1946=EDGE_LOOP('',(#6190,#6191,#6192,#6193));
#1947=EDGE_LOOP('',(#6194));
#1948=EDGE_LOOP('',(#6195));
#1949=EDGE_LOOP('',(#6196,#6197,#6198,#6199));
#1950=EDGE_LOOP('',(#6200,#6201,#6202,#6203));
#1951=EDGE_LOOP('',(#6204,#6205,#6206,#6207,#6208,#6209));
#1952=EDGE_LOOP('',(#6210,#6211,#6212,#6213,#6214));
#1953=EDGE_LOOP('',(#6215,#6216,#6217,#6218));
#1954=EDGE_LOOP('',(#6219,#6220,#6221,#6222));
#1955=EDGE_LOOP('',(#6223));
#1956=EDGE_LOOP('',(#6224));
#1957=EDGE_LOOP('',(#6225,#6226,#6227,#6228,#6229));
#1958=EDGE_LOOP('',(#6230));
#1959=EDGE_LOOP('',(#6231));
#1960=EDGE_LOOP('',(#6232,#6233,#6234,#6235));
#1961=EDGE_LOOP('',(#6236,#6237,#6238,#6239,#6240,#6241));
#1962=EDGE_LOOP('',(#6242,#6243,#6244,#6245,#6246));
#1963=EDGE_LOOP('',(#6247));
#1964=EDGE_LOOP('',(#6248));
#1965=EDGE_LOOP('',(#6249,#6250,#6251,#6252));
#1966=EDGE_LOOP('',(#6253,#6254,#6255,#6256));
#1967=EDGE_LOOP('',(#6257,#6258,#6259,#6260));
#1968=EDGE_LOOP('',(#6261));
#1969=EDGE_LOOP('',(#6262));
#1970=EDGE_LOOP('',(#6263,#6264,#6265,#6266,#6267));
#1971=EDGE_LOOP('',(#6268,#6269));
#1972=EDGE_LOOP('',(#6270,#6271));
#1973=EDGE_LOOP('',(#6272,#6273));
#1974=EDGE_LOOP('',(#6274,#6275));
#1975=EDGE_LOOP('',(#6276,#6277));
#1976=EDGE_LOOP('',(#6278,#6279));
#1977=EDGE_LOOP('',(#6280,#6281));
#1978=EDGE_LOOP('',(#6282,#6283,#6284,#6285));
#1979=EDGE_LOOP('',(#6286,#6287,#6288,#6289,#6290,#6291,#6292,#6293,#6294,
#6295,#6296,#6297,#6298,#6299,#6300,#6301,#6302,#6303));
#1980=EDGE_LOOP('',(#6304,#6305,#6306,#6307));
#1981=EDGE_LOOP('',(#6308,#6309,#6310,#6311));
#1982=EDGE_LOOP('',(#6312,#6313,#6314,#6315));
#1983=EDGE_LOOP('',(#6316,#6317,#6318,#6319));
#1984=EDGE_LOOP('',(#6320,#6321,#6322,#6323,#6324,#6325));
#1985=EDGE_LOOP('',(#6326,#6327,#6328,#6329));
#1986=EDGE_LOOP('',(#6330,#6331,#6332,#6333));
#1987=EDGE_LOOP('',(#6334,#6335,#6336,#6337));
#1988=EDGE_LOOP('',(#6338,#6339,#6340,#6341));
#1989=EDGE_LOOP('',(#6342,#6343,#6344,#6345));
#1990=EDGE_LOOP('',(#6346,#6347,#6348,#6349,#6350,#6351,#6352,#6353,#6354,
#6355,#6356,#6357,#6358,#6359,#6360,#6361,#6362,#6363));
#1991=EDGE_LOOP('',(#6364,#6365,#6366,#6367));
#1992=EDGE_LOOP('',(#6368,#6369,#6370,#6371));
#1993=EDGE_LOOP('',(#6372));
#1994=EDGE_LOOP('',(#6373));
#1995=EDGE_LOOP('',(#6374,#6375,#6376,#6377));
#1996=EDGE_LOOP('',(#6378));
#1997=EDGE_LOOP('',(#6379));
#1998=EDGE_LOOP('',(#6380,#6381,#6382,#6383));
#1999=EDGE_LOOP('',(#6384));
#2000=EDGE_LOOP('',(#6385));
#2001=EDGE_LOOP('',(#6386,#6387,#6388,#6389));
#2002=EDGE_LOOP('',(#6390));
#2003=EDGE_LOOP('',(#6391));
#2004=EDGE_LOOP('',(#6392,#6393,#6394,#6395));
#2005=EDGE_LOOP('',(#6396));
#2006=EDGE_LOOP('',(#6397));
#2007=EDGE_LOOP('',(#6398,#6399,#6400,#6401));
#2008=EDGE_LOOP('',(#6402,#6403,#6404,#6405,#6406,#6407));
#2009=EDGE_LOOP('',(#6408,#6409,#6410,#6411,#6412));
#2010=EDGE_LOOP('',(#6413,#6414,#6415,#6416));
#2011=EDGE_LOOP('',(#6417,#6418,#6419,#6420));
#2012=EDGE_LOOP('',(#6421));
#2013=EDGE_LOOP('',(#6422));
#2014=EDGE_LOOP('',(#6423,#6424,#6425,#6426,#6427));
#2015=EDGE_LOOP('',(#6428));
#2016=EDGE_LOOP('',(#6429));
#2017=EDGE_LOOP('',(#6430,#6431,#6432,#6433));
#2018=EDGE_LOOP('',(#6434,#6435,#6436,#6437,#6438,#6439));
#2019=EDGE_LOOP('',(#6440,#6441,#6442,#6443,#6444));
#2020=EDGE_LOOP('',(#6445));
#2021=EDGE_LOOP('',(#6446));
#2022=EDGE_LOOP('',(#6447,#6448,#6449,#6450));
#2023=EDGE_LOOP('',(#6451,#6452,#6453,#6454));
#2024=EDGE_LOOP('',(#6455,#6456,#6457,#6458));
#2025=EDGE_LOOP('',(#6459));
#2026=EDGE_LOOP('',(#6460));
#2027=EDGE_LOOP('',(#6461,#6462,#6463,#6464,#6465));
#2028=EDGE_LOOP('',(#6466,#6467));
#2029=EDGE_LOOP('',(#6468,#6469));
#2030=EDGE_LOOP('',(#6470,#6471));
#2031=EDGE_LOOP('',(#6472,#6473));
#2032=EDGE_LOOP('',(#6474,#6475));
#2033=EDGE_LOOP('',(#6476,#6477));
#2034=EDGE_LOOP('',(#6478,#6479));
#2035=EDGE_LOOP('',(#6480,#6481));
#2036=EDGE_LOOP('',(#6482,#6483,#6484,#6485));
#2037=EDGE_LOOP('',(#6486,#6487,#6488,#6489,#6490,#6491,#6492,#6493,#6494,
#6495,#6496,#6497,#6498,#6499,#6500,#6501,#6502,#6503,#6504,#6505));
#2038=EDGE_LOOP('',(#6506,#6507,#6508,#6509));
#2039=EDGE_LOOP('',(#6510,#6511,#6512,#6513));
#2040=EDGE_LOOP('',(#6514,#6515,#6516,#6517));
#2041=EDGE_LOOP('',(#6518,#6519,#6520,#6521));
#2042=EDGE_LOOP('',(#6522,#6523,#6524,#6525));
#2043=EDGE_LOOP('',(#6526,#6527,#6528,#6529,#6530,#6531));
#2044=EDGE_LOOP('',(#6532,#6533,#6534,#6535));
#2045=EDGE_LOOP('',(#6536,#6537,#6538,#6539));
#2046=EDGE_LOOP('',(#6540,#6541,#6542,#6543));
#2047=EDGE_LOOP('',(#6544,#6545,#6546,#6547));
#2048=EDGE_LOOP('',(#6548,#6549,#6550,#6551));
#2049=EDGE_LOOP('',(#6552,#6553,#6554,#6555));
#2050=EDGE_LOOP('',(#6556,#6557,#6558,#6559,#6560,#6561,#6562,#6563,#6564,
#6565,#6566,#6567,#6568,#6569,#6570,#6571,#6572,#6573,#6574,#6575));
#2051=EDGE_LOOP('',(#6576,#6577,#6578,#6579));
#2052=EDGE_LOOP('',(#6580,#6581,#6582,#6583));
#2053=EDGE_LOOP('',(#6584));
#2054=EDGE_LOOP('',(#6585));
#2055=EDGE_LOOP('',(#6586,#6587,#6588,#6589));
#2056=EDGE_LOOP('',(#6590));
#2057=EDGE_LOOP('',(#6591));
#2058=EDGE_LOOP('',(#6592,#6593,#6594,#6595));
#2059=EDGE_LOOP('',(#6596));
#2060=EDGE_LOOP('',(#6597));
#2061=EDGE_LOOP('',(#6598,#6599,#6600,#6601));
#2062=EDGE_LOOP('',(#6602));
#2063=EDGE_LOOP('',(#6603));
#2064=EDGE_LOOP('',(#6604,#6605,#6606,#6607));
#2065=EDGE_LOOP('',(#6608));
#2066=EDGE_LOOP('',(#6609));
#2067=EDGE_LOOP('',(#6610,#6611,#6612,#6613));
#2068=EDGE_LOOP('',(#6614));
#2069=EDGE_LOOP('',(#6615,#6616,#6617,#6618));
#2070=EDGE_LOOP('',(#6619,#6620,#6621,#6622));
#2071=EDGE_LOOP('',(#6623,#6624,#6625,#6626));
#2072=EDGE_LOOP('',(#6627));
#2073=EDGE_LOOP('',(#6628));
#2074=EDGE_LOOP('',(#6629,#6630,#6631,#6632));
#2075=EDGE_LOOP('',(#6633,#6634,#6635,#6636));
#2076=EDGE_LOOP('',(#6637,#6638,#6639,#6640));
#2077=EDGE_LOOP('',(#6641));
#2078=EDGE_LOOP('',(#6642,#6643,#6644,#6645));
#2079=EDGE_LOOP('',(#6646,#6647,#6648,#6649));
#2080=EDGE_LOOP('',(#6650,#6651,#6652,#6653));
#2081=EDGE_LOOP('',(#6654,#6655,#6656,#6657));
#2082=EDGE_LOOP('',(#6658,#6659,#6660,#6661));
#2083=EDGE_LOOP('',(#6662,#6663,#6664,#6665));
#2084=EDGE_LOOP('',(#6666,#6667,#6668,#6669,#6670,#6671));
#2085=EDGE_LOOP('',(#6672,#6673,#6674,#6675,#6676,#6677));
#2086=EDGE_LOOP('',(#6678,#6679,#6680,#6681));
#2087=EDGE_LOOP('',(#6682,#6683,#6684,#6685));
#2088=EDGE_LOOP('',(#6686,#6687,#6688,#6689));
#2089=EDGE_LOOP('',(#6690,#6691,#6692,#6693));
#2090=EDGE_LOOP('',(#6694,#6695,#6696,#6697));
#2091=EDGE_LOOP('',(#6698,#6699,#6700,#6701));
#2092=EDGE_LOOP('',(#6702,#6703,#6704,#6705,#6706,#6707));
#2093=EDGE_LOOP('',(#6708,#6709,#6710,#6711,#6712,#6713));
#2094=EDGE_LOOP('',(#6714));
#2095=EDGE_LOOP('',(#6715));
#2096=EDGE_LOOP('',(#6716,#6717,#6718,#6719));
#2097=EDGE_LOOP('',(#6720,#6721,#6722,#6723));
#2098=EDGE_LOOP('',(#6724,#6725,#6726,#6727));
#2099=EDGE_LOOP('',(#6728));
#2100=EDGE_LOOP('',(#6729));
#2101=EDGE_LOOP('',(#6730,#6731,#6732,#6733));
#2102=EDGE_LOOP('',(#6734,#6735,#6736,#6737));
#2103=EDGE_LOOP('',(#6738,#6739,#6740,#6741));
#2104=EDGE_LOOP('',(#6742));
#2105=EDGE_LOOP('',(#6743,#6744,#6745,#6746));
#2106=EDGE_LOOP('',(#6747));
#2107=EDGE_LOOP('',(#6748,#6749,#6750,#6751));
#2108=EDGE_LOOP('',(#6752));
#2109=EDGE_LOOP('',(#6753));
#2110=EDGE_LOOP('',(#6754));
#2111=EDGE_LOOP('',(#6755));
#2112=EDGE_LOOP('',(#6756,#6757,#6758,#6759));
#2113=EDGE_LOOP('',(#6760,#6761,#6762,#6763));
#2114=EDGE_LOOP('',(#6764));
#2115=EDGE_LOOP('',(#6765));
#2116=EDGE_LOOP('',(#6766));
#2117=EDGE_LOOP('',(#6767));
#2118=EDGE_LOOP('',(#6768,#6769,#6770,#6771));
#2119=EDGE_LOOP('',(#6772,#6773,#6774,#6775));
#2120=EDGE_LOOP('',(#6776));
#2121=EDGE_LOOP('',(#6777));
#2122=EDGE_LOOP('',(#6778));
#2123=EDGE_LOOP('',(#6779));
#2124=EDGE_LOOP('',(#6780,#6781));
#2125=EDGE_LOOP('',(#6782,#6783,#6784,#6785,#6786,#6787,#6788,#6789,#6790));
#2126=EDGE_LOOP('',(#6791,#6792,#6793));
#2127=EDGE_LOOP('',(#6794,#6795,#6796,#6797));
#2128=EDGE_LOOP('',(#6798,#6799,#6800,#6801));
#2129=EDGE_LOOP('',(#6802,#6803,#6804,#6805));
#2130=EDGE_LOOP('',(#6806,#6807));
#2131=EDGE_LOOP('',(#6808));
#2132=EDGE_LOOP('',(#6809));
#2133=EDGE_LOOP('',(#6810));
#2134=EDGE_LOOP('',(#6811));
#2135=EDGE_LOOP('',(#6812,#6813));
#2136=EDGE_LOOP('',(#6814,#6815,#6816,#6817,#6818,#6819,#6820,#6821,#6822));
#2137=EDGE_LOOP('',(#6823,#6824,#6825));
#2138=EDGE_LOOP('',(#6826,#6827,#6828,#6829));
#2139=EDGE_LOOP('',(#6830,#6831,#6832,#6833));
#2140=EDGE_LOOP('',(#6834,#6835,#6836,#6837));
#2141=EDGE_LOOP('',(#6838,#6839));
#2142=EDGE_LOOP('',(#6840));
#2143=EDGE_LOOP('',(#6841));
#2144=EDGE_LOOP('',(#6842));
#2145=EDGE_LOOP('',(#6843));
#2146=EDGE_LOOP('',(#6844,#6845,#6846,#6847));
#2147=EDGE_LOOP('',(#6848,#6849,#6850,#6851));
#2148=EDGE_LOOP('',(#6852));
#2149=EDGE_LOOP('',(#6853));
#2150=EDGE_LOOP('',(#6854));
#2151=EDGE_LOOP('',(#6855));
#2152=EDGE_LOOP('',(#6856,#6857,#6858,#6859));
#2153=EDGE_LOOP('',(#6860,#6861,#6862,#6863));
#2154=EDGE_LOOP('',(#6864));
#2155=EDGE_LOOP('',(#6865));
#2156=EDGE_LOOP('',(#6866));
#2157=EDGE_LOOP('',(#6867));
#2158=EDGE_LOOP('',(#6868,#6869));
#2159=EDGE_LOOP('',(#6870,#6871,#6872,#6873,#6874,#6875,#6876,#6877,#6878));
#2160=EDGE_LOOP('',(#6879,#6880,#6881));
#2161=EDGE_LOOP('',(#6882,#6883,#6884,#6885));
#2162=EDGE_LOOP('',(#6886,#6887,#6888,#6889));
#2163=EDGE_LOOP('',(#6890,#6891,#6892,#6893));
#2164=EDGE_LOOP('',(#6894,#6895));
#2165=EDGE_LOOP('',(#6896));
#2166=EDGE_LOOP('',(#6897));
#2167=EDGE_LOOP('',(#6898));
#2168=EDGE_LOOP('',(#6899));
#2169=EDGE_LOOP('',(#6900,#6901));
#2170=EDGE_LOOP('',(#6902,#6903,#6904,#6905,#6906,#6907,#6908,#6909,#6910));
#2171=EDGE_LOOP('',(#6911,#6912,#6913));
#2172=EDGE_LOOP('',(#6914,#6915,#6916,#6917));
#2173=EDGE_LOOP('',(#6918,#6919,#6920,#6921));
#2174=EDGE_LOOP('',(#6922,#6923,#6924,#6925));
#2175=EDGE_LOOP('',(#6926,#6927));
#2176=EDGE_LOOP('',(#6928));
#2177=EDGE_LOOP('',(#6929));
#2178=EDGE_LOOP('',(#6930));
#2179=EDGE_LOOP('',(#6931));
#2180=EDGE_LOOP('',(#6932,#6933));
#2181=EDGE_LOOP('',(#6934,#6935,#6936,#6937,#6938,#6939,#6940,#6941,#6942));
#2182=EDGE_LOOP('',(#6943,#6944,#6945));
#2183=EDGE_LOOP('',(#6946,#6947,#6948,#6949));
#2184=EDGE_LOOP('',(#6950,#6951,#6952,#6953));
#2185=EDGE_LOOP('',(#6954,#6955,#6956,#6957));
#2186=EDGE_LOOP('',(#6958,#6959,#6960,#6961));
#2187=EDGE_LOOP('',(#6962));
#2188=EDGE_LOOP('',(#6963));
#2189=EDGE_LOOP('',(#6964));
#2190=EDGE_LOOP('',(#6965));
#2191=EDGE_LOOP('',(#6966));
#2192=EDGE_LOOP('',(#6967));
#2193=EDGE_LOOP('',(#6968,#6969,#6970,#6971));
#2194=EDGE_LOOP('',(#6972,#6973,#6974,#6975));
#2195=EDGE_LOOP('',(#6976,#6977,#6978,#6979));
#2196=EDGE_LOOP('',(#6980,#6981,#6982,#6983));
#2197=EDGE_LOOP('',(#6984,#6985));
#2198=EDGE_LOOP('',(#6986));
#2199=EDGE_LOOP('',(#6987));
#2200=EDGE_LOOP('',(#6988));
#2201=EDGE_LOOP('',(#6989));
#2202=EDGE_LOOP('',(#6990));
#2203=EDGE_LOOP('',(#6991));
#2204=EDGE_LOOP('',(#6992));
#2205=EDGE_LOOP('',(#6993));
#2206=EDGE_LOOP('',(#6994,#6995,#6996,#6997));
#2207=EDGE_LOOP('',(#6998,#6999,#7000,#7001));
#2208=EDGE_LOOP('',(#7002,#7003,#7004,#7005));
#2209=EDGE_LOOP('',(#7006,#7007,#7008,#7009));
#2210=EDGE_LOOP('',(#7010,#7011,#7012,#7013));
#2211=EDGE_LOOP('',(#7014,#7015,#7016,#7017));
#2212=EDGE_LOOP('',(#7018,#7019,#7020,#7021,#7022,#7023));
#2213=EDGE_LOOP('',(#7024));
#2214=EDGE_LOOP('',(#7025,#7026,#7027,#7028,#7029,#7030));
#2215=EDGE_LOOP('',(#7031,#7032,#7033,#7034));
#2216=EDGE_LOOP('',(#7035,#7036,#7037,#7038));
#2217=EDGE_LOOP('',(#7039,#7040,#7041,#7042));
#2218=EDGE_LOOP('',(#7043));
#2219=LINE('',#11665,#2663);
#2220=LINE('',#11671,#2664);
#2221=LINE('',#11677,#2665);
#2222=LINE('',#11683,#2666);
#2223=LINE('',#11689,#2667);
#2224=LINE('',#11695,#2668);
#2225=LINE('',#11701,#2669);
#2226=LINE('',#11707,#2670);
#2227=LINE('',#11713,#2671);
#2228=LINE('',#11719,#2672);
#2229=LINE('',#11725,#2673);
#2230=LINE('',#11731,#2674);
#2231=LINE('',#11736,#2675);
#2232=LINE('',#11738,#2676);
#2233=LINE('',#11740,#2677);
#2234=LINE('',#11741,#2678);
#2235=LINE('',#11744,#2679);
#2236=LINE('',#11746,#2680);
#2237=LINE('',#11747,#2681);
#2238=LINE('',#11750,#2682);
#2239=LINE('',#11752,#2683);
#2240=LINE('',#11753,#2684);
#2241=LINE('',#11755,#2685);
#2242=LINE('',#11756,#2686);
#2243=LINE('',#11764,#2687);
#2244=LINE('',#11770,#2688);
#2245=LINE('',#11776,#2689);
#2246=LINE('',#11782,#2690);
#2247=LINE('',#11787,#2691);
#2248=LINE('',#11793,#2692);
#2249=LINE('',#11802,#2693);
#2250=LINE('',#11809,#2694);
#2251=LINE('',#11817,#2695);
#2252=LINE('',#11821,#2696);
#2253=LINE('',#11825,#2697);
#2254=LINE('',#11827,#2698);
#2255=LINE('',#11829,#2699);
#2256=LINE('',#11830,#2700);
#2257=LINE('',#11834,#2701);
#2258=LINE('',#11836,#2702);
#2259=LINE('',#11838,#2703);
#2260=LINE('',#11839,#2704);
#2261=LINE('',#11842,#2705);
#2262=LINE('',#11844,#2706);
#2263=LINE('',#11845,#2707);
#2264=LINE('',#11848,#2708);
#2265=LINE('',#11850,#2709);
#2266=LINE('',#11851,#2710);
#2267=LINE('',#11853,#2711);
#2268=LINE('',#11854,#2712);
#2269=LINE('',#11861,#2713);
#2270=LINE('',#11871,#2714);
#2271=LINE('',#11877,#2715);
#2272=LINE('',#11883,#2716);
#2273=LINE('',#11889,#2717);
#2274=LINE('',#11895,#2718);
#2275=LINE('',#11902,#2719);
#2276=LINE('',#11908,#2720);
#2277=LINE('',#11917,#2721);
#2278=LINE('',#11923,#2722);
#2279=LINE('',#11929,#2723);
#2280=LINE('',#11935,#2724);
#2281=LINE('',#11941,#2725);
#2282=LINE('',#11949,#2726);
#2283=LINE('',#11954,#2727);
#2284=LINE('',#11963,#2728);
#2285=LINE('',#11969,#2729);
#2286=LINE('',#11975,#2730);
#2287=LINE('',#11981,#2731);
#2288=LINE('',#11986,#2732);
#2289=LINE('',#11992,#2733);
#2290=LINE('',#12001,#2734);
#2291=LINE('',#12008,#2735);
#2292=LINE('',#12016,#2736);
#2293=LINE('',#12020,#2737);
#2294=LINE('',#12024,#2738);
#2295=LINE('',#12026,#2739);
#2296=LINE('',#12028,#2740);
#2297=LINE('',#12029,#2741);
#2298=LINE('',#12033,#2742);
#2299=LINE('',#12035,#2743);
#2300=LINE('',#12037,#2744);
#2301=LINE('',#12038,#2745);
#2302=LINE('',#12041,#2746);
#2303=LINE('',#12043,#2747);
#2304=LINE('',#12044,#2748);
#2305=LINE('',#12047,#2749);
#2306=LINE('',#12049,#2750);
#2307=LINE('',#12050,#2751);
#2308=LINE('',#12052,#2752);
#2309=LINE('',#12053,#2753);
#2310=LINE('',#12060,#2754);
#2311=LINE('',#12070,#2755);
#2312=LINE('',#12076,#2756);
#2313=LINE('',#12082,#2757);
#2314=LINE('',#12088,#2758);
#2315=LINE('',#12094,#2759);
#2316=LINE('',#12101,#2760);
#2317=LINE('',#12107,#2761);
#2318=LINE('',#12116,#2762);
#2319=LINE('',#12122,#2763);
#2320=LINE('',#12128,#2764);
#2321=LINE('',#12134,#2765);
#2322=LINE('',#12140,#2766);
#2323=LINE('',#12148,#2767);
#2324=LINE('',#12153,#2768);
#2325=LINE('',#12162,#2769);
#2326=LINE('',#12168,#2770);
#2327=LINE('',#12174,#2771);
#2328=LINE('',#12180,#2772);
#2329=LINE('',#12185,#2773);
#2330=LINE('',#12187,#2774);
#2331=LINE('',#12189,#2775);
#2332=LINE('',#12190,#2776);
#2333=LINE('',#12195,#2777);
#2334=LINE('',#12196,#2778);
#2335=LINE('',#12201,#2779);
#2336=LINE('',#12202,#2780);
#2337=LINE('',#12204,#2781);
#2338=LINE('',#12205,#2782);
#2339=LINE('',#12211,#2783);
#2340=LINE('',#12217,#2784);
#2341=LINE('',#12226,#2785);
#2342=LINE('',#12232,#2786);
#2343=LINE('',#12238,#2787);
#2344=LINE('',#12244,#2788);
#2345=LINE('',#12250,#2789);
#2346=LINE('',#12257,#2790);
#2347=LINE('',#12263,#2791);
#2348=LINE('',#12272,#2792);
#2349=LINE('',#12278,#2793);
#2350=LINE('',#12284,#2794);
#2351=LINE('',#12290,#2795);
#2352=LINE('',#12296,#2796);
#2353=LINE('',#12304,#2797);
#2354=LINE('',#12309,#2798);
#2355=LINE('',#12318,#2799);
#2356=LINE('',#12325,#2800);
#2357=LINE('',#12332,#2801);
#2358=LINE('',#12341,#2802);
#2359=LINE('',#12350,#2803);
#2360=LINE('',#12359,#2804);
#2361=LINE('',#12367,#2805);
#2362=LINE('',#12371,#2806);
#2363=LINE('',#12375,#2807);
#2364=LINE('',#12379,#2808);
#2365=LINE('',#12383,#2809);
#2366=LINE('',#12385,#2810);
#2367=LINE('',#12387,#2811);
#2368=LINE('',#12388,#2812);
#2369=LINE('',#12391,#2813);
#2370=LINE('',#12393,#2814);
#2371=LINE('',#12394,#2815);
#2372=LINE('',#12397,#2816);
#2373=LINE('',#12399,#2817);
#2374=LINE('',#12400,#2818);
#2375=LINE('',#12402,#2819);
#2376=LINE('',#12403,#2820);
#2377=LINE('',#12411,#2821);
#2378=LINE('',#12417,#2822);
#2379=LINE('',#12422,#2823);
#2380=LINE('',#12424,#2824);
#2381=LINE('',#12426,#2825);
#2382=LINE('',#12427,#2826);
#2383=LINE('',#12430,#2827);
#2384=LINE('',#12432,#2828);
#2385=LINE('',#12433,#2829);
#2386=LINE('',#12436,#2830);
#2387=LINE('',#12438,#2831);
#2388=LINE('',#12439,#2832);
#2389=LINE('',#12443,#2833);
#2390=LINE('',#12445,#2834);
#2391=LINE('',#12447,#2835);
#2392=LINE('',#12448,#2836);
#2393=LINE('',#12451,#2837);
#2394=LINE('',#12453,#2838);
#2395=LINE('',#12454,#2839);
#2396=LINE('',#12456,#2840);
#2397=LINE('',#12458,#2841);
#2398=LINE('',#12459,#2842);
#2399=LINE('',#12462,#2843);
#2400=LINE('',#12463,#2844);
#2401=LINE('',#12465,#2845);
#2402=LINE('',#12466,#2846);
#2403=LINE('',#12474,#2847);
#2404=LINE('',#12482,#2848);
#2405=LINE('',#12488,#2849);
#2406=LINE('',#12490,#2850);
#2407=LINE('',#12492,#2851);
#2408=LINE('',#12493,#2852);
#2409=LINE('',#12496,#2853);
#2410=LINE('',#12500,#2854);
#2411=LINE('',#12502,#2855);
#2412=LINE('',#12504,#2856);
#2413=LINE('',#12506,#2857);
#2414=LINE('',#12508,#2858);
#2415=LINE('',#12510,#2859);
#2416=LINE('',#12511,#2860);
#2417=LINE('',#12514,#2861);
#2418=LINE('',#12516,#2862);
#2419=LINE('',#12518,#2863);
#2420=LINE('',#12520,#2864);
#2421=LINE('',#12522,#2865);
#2422=LINE('',#12523,#2866);
#2423=LINE('',#12528,#2867);
#2424=LINE('',#12536,#2868);
#2425=LINE('',#12541,#2869);
#2426=LINE('',#12543,#2870);
#2427=LINE('',#12544,#2871);
#2428=LINE('',#12547,#2872);
#2429=LINE('',#12551,#2873);
#2430=LINE('',#12552,#2874);
#2431=LINE('',#12555,#2875);
#2432=LINE('',#12556,#2876);
#2433=LINE('',#12561,#2877);
#2434=LINE('',#12569,#2878);
#2435=LINE('',#12574,#2879);
#2436=LINE('',#12576,#2880);
#2437=LINE('',#12577,#2881);
#2438=LINE('',#12580,#2882);
#2439=LINE('',#12584,#2883);
#2440=LINE('',#12586,#2884);
#2441=LINE('',#12587,#2885);
#2442=LINE('',#12589,#2886);
#2443=LINE('',#12594,#2887);
#2444=LINE('',#12602,#2888);
#2445=LINE('',#12608,#2889);
#2446=LINE('',#12610,#2890);
#2447=LINE('',#12612,#2891);
#2448=LINE('',#12613,#2892);
#2449=LINE('',#12616,#2893);
#2450=LINE('',#12620,#2894);
#2451=LINE('',#12621,#2895);
#2452=LINE('',#12623,#2896);
#2453=LINE('',#12624,#2897);
#2454=LINE('',#12627,#2898);
#2455=LINE('',#12628,#2899);
#2456=LINE('',#12632,#2900);
#2457=LINE('',#12634,#2901);
#2458=LINE('',#12636,#2902);
#2459=LINE('',#12637,#2903);
#2460=LINE('',#12640,#2904);
#2461=LINE('',#12642,#2905);
#2462=LINE('',#12643,#2906);
#2463=LINE('',#12646,#2907);
#2464=LINE('',#12648,#2908);
#2465=LINE('',#12649,#2909);
#2466=LINE('',#12651,#2910);
#2467=LINE('',#12652,#2911);
#2468=LINE('',#12655,#2912);
#2469=LINE('',#12656,#2913);
#2470=LINE('',#12659,#2914);
#2471=LINE('',#12662,#2915);
#2472=LINE('',#12663,#2916);
#2473=LINE('',#12667,#2917);
#2474=LINE('',#12670,#2918);
#2475=LINE('',#12676,#2919);
#2476=LINE('',#12678,#2920);
#2477=LINE('',#12680,#2921);
#2478=LINE('',#12681,#2922);
#2479=LINE('',#12684,#2923);
#2480=LINE('',#12686,#2924);
#2481=LINE('',#12687,#2925);
#2482=LINE('',#12690,#2926);
#2483=LINE('',#12692,#2927);
#2484=LINE('',#12693,#2928);
#2485=LINE('',#12695,#2929);
#2486=LINE('',#12696,#2930);
#2487=LINE('',#12703,#2931);
#2488=LINE('',#12705,#2932);
#2489=LINE('',#12707,#2933);
#2490=LINE('',#12708,#2934);
#2491=LINE('',#12711,#2935);
#2492=LINE('',#12713,#2936);
#2493=LINE('',#12714,#2937);
#2494=LINE('',#12717,#2938);
#2495=LINE('',#12719,#2939);
#2496=LINE('',#12720,#2940);
#2497=LINE('',#12722,#2941);
#2498=LINE('',#12723,#2942);
#2499=LINE('',#12730,#2943);
#2500=LINE('',#12732,#2944);
#2501=LINE('',#12734,#2945);
#2502=LINE('',#12735,#2946);
#2503=LINE('',#12738,#2947);
#2504=LINE('',#12740,#2948);
#2505=LINE('',#12741,#2949);
#2506=LINE('',#12744,#2950);
#2507=LINE('',#12746,#2951);
#2508=LINE('',#12747,#2952);
#2509=LINE('',#12750,#2953);
#2510=LINE('',#12752,#2954);
#2511=LINE('',#12753,#2955);
#2512=LINE('',#12756,#2956);
#2513=LINE('',#12758,#2957);
#2514=LINE('',#12759,#2958);
#2515=LINE('',#12761,#2959);
#2516=LINE('',#12762,#2960);
#2517=LINE('',#12774,#2961);
#2518=LINE('',#12778,#2962);
#2519=LINE('',#12782,#2963);
#2520=LINE('',#12789,#2964);
#2521=LINE('',#12791,#2965);
#2522=LINE('',#12806,#2966);
#2523=LINE('',#12812,#2967);
#2524=LINE('',#12816,#2968);
#2525=LINE('',#12822,#2969);
#2526=LINE('',#12827,#2970);
#2527=LINE('',#12842,#2971);
#2528=LINE('',#12851,#2972);
#2529=LINE('',#12855,#2973);
#2530=LINE('',#12859,#2974);
#2531=LINE('',#12862,#2975);
#2532=LINE('',#12998,#2976);
#2533=LINE('',#13251,#2977);
#2534=LINE('',#13293,#2978);
#2535=LINE('',#13298,#2979);
#2536=LINE('',#13307,#2980);
#2537=LINE('',#13312,#2981);
#2538=LINE('',#13332,#2982);
#2539=LINE('',#13338,#2983);
#2540=LINE('',#13342,#2984);
#2541=LINE('',#13348,#2985);
#2542=LINE('',#13353,#2986);
#2543=LINE('',#13368,#2987);
#2544=LINE('',#13377,#2988);
#2545=LINE('',#13381,#2989);
#2546=LINE('',#13385,#2990);
#2547=LINE('',#13388,#2991);
#2548=LINE('',#13541,#2992);
#2549=LINE('',#13837,#2993);
#2550=LINE('',#13879,#2994);
#2551=LINE('',#13884,#2995);
#2552=LINE('',#13893,#2996);
#2553=LINE('',#13898,#2997);
#2554=LINE('',#13911,#2998);
#2555=LINE('',#13915,#2999);
#2556=LINE('',#13919,#3000);
#2557=LINE('',#13926,#3001);
#2558=LINE('',#13930,#3002);
#2559=LINE('',#13934,#3003);
#2560=LINE('',#13939,#3004);
#2561=LINE('',#13941,#3005);
#2562=LINE('',#13943,#3006);
#2563=LINE('',#13944,#3007);
#2564=LINE('',#13947,#3008);
#2565=LINE('',#13949,#3009);
#2566=LINE('',#13950,#3010);
#2567=LINE('',#13953,#3011);
#2568=LINE('',#13955,#3012);
#2569=LINE('',#13956,#3013);
#2570=LINE('',#13959,#3014);
#2571=LINE('',#13961,#3015);
#2572=LINE('',#13962,#3016);
#2573=LINE('',#13965,#3017);
#2574=LINE('',#13967,#3018);
#2575=LINE('',#13968,#3019);
#2576=LINE('',#13970,#3020);
#2577=LINE('',#13971,#3021);
#2578=LINE('',#13978,#3022);
#2579=LINE('',#13980,#3023);
#2580=LINE('',#13982,#3024);
#2581=LINE('',#13983,#3025);
#2582=LINE('',#13986,#3026);
#2583=LINE('',#13988,#3027);
#2584=LINE('',#13989,#3028);
#2585=LINE('',#13992,#3029);
#2586=LINE('',#13994,#3030);
#2587=LINE('',#13995,#3031);
#2588=LINE('',#13998,#3032);
#2589=LINE('',#14000,#3033);
#2590=LINE('',#14001,#3034);
#2591=LINE('',#14004,#3035);
#2592=LINE('',#14006,#3036);
#2593=LINE('',#14007,#3037);
#2594=LINE('',#14009,#3038);
#2595=LINE('',#14010,#3039);
#2596=LINE('',#14022,#3040);
#2597=LINE('',#14026,#3041);
#2598=LINE('',#14030,#3042);
#2599=LINE('',#14037,#3043);
#2600=LINE('',#14039,#3044);
#2601=LINE('',#14102,#3045);
#2602=LINE('',#14109,#3046);
#2603=LINE('',#14116,#3047);
#2604=LINE('',#14125,#3048);
#2605=LINE('',#14131,#3049);
#2606=LINE('',#14140,#3050);
#2607=LINE('',#14146,#3051);
#2608=LINE('',#14154,#3052);
#2609=LINE('',#14171,#3053);
#2610=LINE('',#14222,#3054);
#2611=LINE('',#14227,#3055);
#2612=LINE('',#14233,#3056);
#2613=LINE('',#14241,#3057);
#2614=LINE('',#14258,#3058);
#2615=LINE('',#14309,#3059);
#2616=LINE('',#14314,#3060);
#2617=LINE('',#14320,#3061);
#2618=LINE('',#14329,#3062);
#2619=LINE('',#14335,#3063);
#2620=LINE('',#14344,#3064);
#2621=LINE('',#14350,#3065);
#2622=LINE('',#14358,#3066);
#2623=LINE('',#14379,#3067);
#2624=LINE('',#14434,#3068);
#2625=LINE('',#14439,#3069);
#2626=LINE('',#14445,#3070);
#2627=LINE('',#14453,#3071);
#2628=LINE('',#14474,#3072);
#2629=LINE('',#14529,#3073);
#2630=LINE('',#14534,#3074);
#2631=LINE('',#14540,#3075);
#2632=LINE('',#14548,#3076);
#2633=LINE('',#14565,#3077);
#2634=LINE('',#14616,#3078);
#2635=LINE('',#14621,#3079);
#2636=LINE('',#14627,#3080);
#2637=LINE('',#14633,#3081);
#2638=LINE('',#14639,#3082);
#2639=LINE('',#14648,#3083);
#2640=LINE('',#14654,#3084);
#2641=LINE('',#14659,#3085);
#2642=LINE('',#14666,#3086);
#2643=LINE('',#14668,#3087);
#2644=LINE('',#14670,#3088);
#2645=LINE('',#14671,#3089);
#2646=LINE('',#14674,#3090);
#2647=LINE('',#14676,#3091);
#2648=LINE('',#14677,#3092);
#2649=LINE('',#14680,#3093);
#2650=LINE('',#14682,#3094);
#2651=LINE('',#14683,#3095);
#2652=LINE('',#14686,#3096);
#2653=LINE('',#14688,#3097);
#2654=LINE('',#14689,#3098);
#2655=LINE('',#14692,#3099);
#2656=LINE('',#14694,#3100);
#2657=LINE('',#14695,#3101);
#2658=LINE('',#14697,#3102);
#2659=LINE('',#14698,#3103);
#2660=LINE('',#14706,#3104);
#2661=LINE('',#14710,#3105);
#2662=LINE('',#14714,#3106);
#2663=VECTOR('',#9176,0.165);
#2664=VECTOR('',#9183,0.165);
#2665=VECTOR('',#9190,0.165);
#2666=VECTOR('',#9197,0.165);
#2667=VECTOR('',#9204,0.210000000000001);
#2668=VECTOR('',#9211,0.210000000000001);
#2669=VECTOR('',#9218,0.210000000000001);
#2670=VECTOR('',#9225,0.210000000000001);
#2671=VECTOR('',#9232,0.25);
#2672=VECTOR('',#9239,0.25);
#2673=VECTOR('',#9246,0.25);
#2674=VECTOR('',#9253,0.25);
#2675=VECTOR('',#9258,1.);
#2676=VECTOR('',#9259,1.);
#2677=VECTOR('',#9260,1.);
#2678=VECTOR('',#9261,1.);
#2679=VECTOR('',#9264,1.);
#2680=VECTOR('',#9265,1.);
#2681=VECTOR('',#9266,1.);
#2682=VECTOR('',#9269,1.);
#2683=VECTOR('',#9270,1.);
#2684=VECTOR('',#9271,1.);
#2685=VECTOR('',#9274,1.);
#2686=VECTOR('',#9275,1.);
#2687=VECTOR('',#9286,0.165);
#2688=VECTOR('',#9293,0.165);
#2689=VECTOR('',#9300,0.165);
#2690=VECTOR('',#9307,0.165);
#2691=VECTOR('',#9312,1.);
#2692=VECTOR('',#9319,0.6);
#2693=VECTOR('',#9330,1.);
#2694=VECTOR('',#9339,0.6);
#2695=VECTOR('',#9350,0.33);
#2696=VECTOR('',#9355,0.33);
#2697=VECTOR('',#9358,1.);
#2698=VECTOR('',#9359,1.);
#2699=VECTOR('',#9360,1.);
#2700=VECTOR('',#9361,1.);
#2701=VECTOR('',#9364,1.);
#2702=VECTOR('',#9365,1.);
#2703=VECTOR('',#9366,1.);
#2704=VECTOR('',#9367,1.);
#2705=VECTOR('',#9370,1.);
#2706=VECTOR('',#9371,1.);
#2707=VECTOR('',#9372,1.);
#2708=VECTOR('',#9375,1.);
#2709=VECTOR('',#9376,1.);
#2710=VECTOR('',#9377,1.);
#2711=VECTOR('',#9380,1.);
#2712=VECTOR('',#9381,1.);
#2713=VECTOR('',#9390,1.6);
#2714=VECTOR('',#9405,0.225);
#2715=VECTOR('',#9412,0.225);
#2716=VECTOR('',#9419,0.225);
#2717=VECTOR('',#9426,0.225);
#2718=VECTOR('',#9433,1.59);
#2719=VECTOR('',#9442,1.1);
#2720=VECTOR('',#9449,2.5);
#2721=VECTOR('',#9462,0.225);
#2722=VECTOR('',#9469,0.225);
#2723=VECTOR('',#9476,0.225);
#2724=VECTOR('',#9483,0.225);
#2725=VECTOR('',#9490,1.59);
#2726=VECTOR('',#9501,1.1);
#2727=VECTOR('',#9506,2.5);
#2728=VECTOR('',#9519,0.165);
#2729=VECTOR('',#9526,0.165);
#2730=VECTOR('',#9533,0.165);
#2731=VECTOR('',#9540,0.165);
#2732=VECTOR('',#9545,1.);
#2733=VECTOR('',#9552,0.6);
#2734=VECTOR('',#9563,1.);
#2735=VECTOR('',#9572,0.6);
#2736=VECTOR('',#9583,0.33);
#2737=VECTOR('',#9588,0.33);
#2738=VECTOR('',#9591,1.);
#2739=VECTOR('',#9592,1.);
#2740=VECTOR('',#9593,1.);
#2741=VECTOR('',#9594,1.);
#2742=VECTOR('',#9597,1.);
#2743=VECTOR('',#9598,1.);
#2744=VECTOR('',#9599,1.);
#2745=VECTOR('',#9600,1.);
#2746=VECTOR('',#9603,1.);
#2747=VECTOR('',#9604,1.);
#2748=VECTOR('',#9605,1.);
#2749=VECTOR('',#9608,1.);
#2750=VECTOR('',#9609,1.);
#2751=VECTOR('',#9610,1.);
#2752=VECTOR('',#9613,1.);
#2753=VECTOR('',#9614,1.);
#2754=VECTOR('',#9623,1.6);
#2755=VECTOR('',#9638,0.225);
#2756=VECTOR('',#9645,0.225);
#2757=VECTOR('',#9652,0.225);
#2758=VECTOR('',#9659,0.225);
#2759=VECTOR('',#9666,1.59);
#2760=VECTOR('',#9675,1.1);
#2761=VECTOR('',#9682,2.5);
#2762=VECTOR('',#9695,0.225);
#2763=VECTOR('',#9702,0.225);
#2764=VECTOR('',#9709,0.225);
#2765=VECTOR('',#9716,0.225);
#2766=VECTOR('',#9723,1.59);
#2767=VECTOR('',#9734,1.1);
#2768=VECTOR('',#9739,2.5);
#2769=VECTOR('',#9752,0.165);
#2770=VECTOR('',#9759,0.165);
#2771=VECTOR('',#9766,0.165);
#2772=VECTOR('',#9773,0.165);
#2773=VECTOR('',#9778,1.);
#2774=VECTOR('',#9779,1.);
#2775=VECTOR('',#9780,1.);
#2776=VECTOR('',#9781,1.);
#2777=VECTOR('',#9786,1.);
#2778=VECTOR('',#9787,1.);
#2779=VECTOR('',#9792,1.);
#2780=VECTOR('',#9793,1.);
#2781=VECTOR('',#9796,1.);
#2782=VECTOR('',#9797,1.);
#2783=VECTOR('',#9804,2.35);
#2784=VECTOR('',#9811,3.);
#2785=VECTOR('',#9824,0.225);
#2786=VECTOR('',#9831,0.225);
#2787=VECTOR('',#9838,0.225);
#2788=VECTOR('',#9845,0.225);
#2789=VECTOR('',#9852,2.34);
#2790=VECTOR('',#9861,1.9);
#2791=VECTOR('',#9868,3.);
#2792=VECTOR('',#9881,0.225);
#2793=VECTOR('',#9888,0.225);
#2794=VECTOR('',#9895,0.225);
#2795=VECTOR('',#9902,0.225);
#2796=VECTOR('',#9909,2.34);
#2797=VECTOR('',#9920,1.9);
#2798=VECTOR('',#9925,3.);
#2799=VECTOR('',#9938,0.164999999999999);
#2800=VECTOR('',#9947,0.164999999999999);
#2801=VECTOR('',#9956,0.5);
#2802=VECTOR('',#9967,0.5);
#2803=VECTOR('',#9978,0.5);
#2804=VECTOR('',#9989,0.5);
#2805=VECTOR('',#10000,0.275);
#2806=VECTOR('',#10005,0.275);
#2807=VECTOR('',#10010,0.275);
#2808=VECTOR('',#10015,0.275);
#2809=VECTOR('',#10018,1.);
#2810=VECTOR('',#10019,1.);
#2811=VECTOR('',#10020,1.);
#2812=VECTOR('',#10021,1.);
#2813=VECTOR('',#10024,1.);
#2814=VECTOR('',#10025,1.);
#2815=VECTOR('',#10026,1.);
#2816=VECTOR('',#10029,1.);
#2817=VECTOR('',#10030,1.);
#2818=VECTOR('',#10031,1.);
#2819=VECTOR('',#10034,1.);
#2820=VECTOR('',#10035,1.);
#2821=VECTOR('',#10046,0.225);
#2822=VECTOR('',#10053,0.225);
#2823=VECTOR('',#10058,1.);
#2824=VECTOR('',#10059,1.);
#2825=VECTOR('',#10060,1.);
#2826=VECTOR('',#10061,1.);
#2827=VECTOR('',#10064,1.);
#2828=VECTOR('',#10065,1.);
#2829=VECTOR('',#10066,1.);
#2830=VECTOR('',#10069,1.);
#2831=VECTOR('',#10070,1.);
#2832=VECTOR('',#10071,1.);
#2833=VECTOR('',#10074,1.);
#2834=VECTOR('',#10075,1.);
#2835=VECTOR('',#10076,1.);
#2836=VECTOR('',#10077,1.);
#2837=VECTOR('',#10080,1.);
#2838=VECTOR('',#10081,1.);
#2839=VECTOR('',#10082,1.);
#2840=VECTOR('',#10085,1.);
#2841=VECTOR('',#10086,1.);
#2842=VECTOR('',#10087,1.);
#2843=VECTOR('',#10090,1.);
#2844=VECTOR('',#10091,1.);
#2845=VECTOR('',#10094,1.);
#2846=VECTOR('',#10095,1.);
#2847=VECTOR('',#10106,0.4);
#2848=VECTOR('',#10117,0.225);
#2849=VECTOR('',#10122,1.);
#2850=VECTOR('',#10123,1.);
#2851=VECTOR('',#10124,1.);
#2852=VECTOR('',#10125,1.);
#2853=VECTOR('',#10128,0.9);
#2854=VECTOR('',#10133,1.);
#2855=VECTOR('',#10134,1.);
#2856=VECTOR('',#10135,1.);
#2857=VECTOR('',#10136,1.);
#2858=VECTOR('',#10137,1.);
#2859=VECTOR('',#10138,1.);
#2860=VECTOR('',#10139,1.);
#2861=VECTOR('',#10142,1.);
#2862=VECTOR('',#10143,1.);
#2863=VECTOR('',#10144,1.);
#2864=VECTOR('',#10145,1.);
#2865=VECTOR('',#10146,1.);
#2866=VECTOR('',#10147,1.);
#2867=VECTOR('',#10152,0.4);
#2868=VECTOR('',#10163,0.225);
#2869=VECTOR('',#10168,1.);
#2870=VECTOR('',#10169,1.);
#2871=VECTOR('',#10170,1.);
#2872=VECTOR('',#10173,0.9);
#2873=VECTOR('',#10178,1.);
#2874=VECTOR('',#10179,1.);
#2875=VECTOR('',#10182,1.);
#2876=VECTOR('',#10183,1.);
#2877=VECTOR('',#10188,0.4);
#2878=VECTOR('',#10199,0.225);
#2879=VECTOR('',#10204,1.);
#2880=VECTOR('',#10205,1.);
#2881=VECTOR('',#10206,1.);
#2882=VECTOR('',#10209,0.9);
#2883=VECTOR('',#10214,1.);
#2884=VECTOR('',#10215,1.);
#2885=VECTOR('',#10216,1.);
#2886=VECTOR('',#10219,1.);
#2887=VECTOR('',#10224,0.4);
#2888=VECTOR('',#10235,0.225);
#2889=VECTOR('',#10240,1.);
#2890=VECTOR('',#10241,1.);
#2891=VECTOR('',#10242,1.);
#2892=VECTOR('',#10243,1.);
#2893=VECTOR('',#10246,0.9);
#2894=VECTOR('',#10251,1.);
#2895=VECTOR('',#10252,1.);
#2896=VECTOR('',#10253,1.);
#2897=VECTOR('',#10254,1.);
#2898=VECTOR('',#10257,1.);
#2899=VECTOR('',#10258,1.);
#2900=VECTOR('',#10261,1.);
#2901=VECTOR('',#10262,1.);
#2902=VECTOR('',#10263,1.);
#2903=VECTOR('',#10264,1.);
#2904=VECTOR('',#10267,1.);
#2905=VECTOR('',#10268,1.);
#2906=VECTOR('',#10269,1.);
#2907=VECTOR('',#10272,1.);
#2908=VECTOR('',#10273,1.);
#2909=VECTOR('',#10274,1.);
#2910=VECTOR('',#10277,1.);
#2911=VECTOR('',#10278,1.);
#2912=VECTOR('',#10281,1.);
#2913=VECTOR('',#10282,1.);
#2914=VECTOR('',#10287,1.);
#2915=VECTOR('',#10290,1.);
#2916=VECTOR('',#10291,1.);
#2917=VECTOR('',#10298,1.);
#2918=VECTOR('',#10303,1.);
#2919=VECTOR('',#10310,1.);
#2920=VECTOR('',#10311,1.);
#2921=VECTOR('',#10312,1.);
#2922=VECTOR('',#10313,1.);
#2923=VECTOR('',#10316,1.);
#2924=VECTOR('',#10317,1.);
#2925=VECTOR('',#10318,1.);
#2926=VECTOR('',#10321,1.);
#2927=VECTOR('',#10322,1.);
#2928=VECTOR('',#10323,1.);
#2929=VECTOR('',#10326,1.);
#2930=VECTOR('',#10327,1.);
#2931=VECTOR('',#10336,1.);
#2932=VECTOR('',#10337,1.);
#2933=VECTOR('',#10338,1.);
#2934=VECTOR('',#10339,1.);
#2935=VECTOR('',#10342,1.);
#2936=VECTOR('',#10343,1.);
#2937=VECTOR('',#10344,1.);
#2938=VECTOR('',#10347,1.);
#2939=VECTOR('',#10348,1.);
#2940=VECTOR('',#10349,1.);
#2941=VECTOR('',#10352,1.);
#2942=VECTOR('',#10353,1.);
#2943=VECTOR('',#10362,1.);
#2944=VECTOR('',#10363,1.);
#2945=VECTOR('',#10364,1.);
#2946=VECTOR('',#10365,1.);
#2947=VECTOR('',#10368,1.);
#2948=VECTOR('',#10369,1.);
#2949=VECTOR('',#10370,1.);
#2950=VECTOR('',#10373,1.);
#2951=VECTOR('',#10374,1.);
#2952=VECTOR('',#10375,1.);
#2953=VECTOR('',#10378,1.);
#2954=VECTOR('',#10379,1.);
#2955=VECTOR('',#10380,1.);
#2956=VECTOR('',#10383,1.);
#2957=VECTOR('',#10384,1.);
#2958=VECTOR('',#10385,1.);
#2959=VECTOR('',#10388,1.);
#2960=VECTOR('',#10389,1.);
#2961=VECTOR('',#10406,0.475);
#2962=VECTOR('',#10411,0.5);
#2963=VECTOR('',#10416,0.485);
#2964=VECTOR('',#10425,0.31);
#2965=VECTOR('',#10428,0.3);
#2966=VECTOR('',#10447,1.070235);
#2967=VECTOR('',#10454,0.6);
#2968=VECTOR('',#10459,0.63);
#2969=VECTOR('',#10468,1.070235);
#2970=VECTOR('',#10475,0.63);
#2971=VECTOR('',#10494,1.129765);
#2972=VECTOR('',#10505,1.57);
#2973=VECTOR('',#10510,1.6);
#2974=VECTOR('',#10515,1.57);
#2975=VECTOR('',#10520,1.129765);
#2976=VECTOR('',#10567,1.123812);
#2977=VECTOR('',#10636,1.076188);
#2978=VECTOR('',#10665,1.119765);
#2979=VECTOR('',#10672,1.085235);
#2980=VECTOR('',#10683,1.119765);
#2981=VECTOR('',#10690,1.085235);
#2982=VECTOR('',#10719,1.63531);
#2983=VECTOR('',#10726,1.);
#2984=VECTOR('',#10731,1.05);
#2985=VECTOR('',#10740,1.63531);
#2986=VECTOR('',#10747,1.05);
#2987=VECTOR('',#10766,1.71469);
#2988=VECTOR('',#10777,2.3);
#2989=VECTOR('',#10782,2.35);
#2990=VECTOR('',#10787,2.3);
#2991=VECTOR('',#10792,1.71469);
#2992=VECTOR('',#10843,1.706752);
#2993=VECTOR('',#10920,1.643248);
#2994=VECTOR('',#10949,1.70469);
#2995=VECTOR('',#10956,1.65031);
#2996=VECTOR('',#10967,1.70469);
#2997=VECTOR('',#10974,1.65031);
#2998=VECTOR('',#10995,0.4);
#2999=VECTOR('',#11000,0.425);
#3000=VECTOR('',#11005,0.41);
#3001=VECTOR('',#11014,0.26);
#3002=VECTOR('',#11019,0.25);
#3003=VECTOR('',#11024,0.225);
#3004=VECTOR('',#11029,1.);
#3005=VECTOR('',#11030,1.);
#3006=VECTOR('',#11031,1.);
#3007=VECTOR('',#11032,1.);
#3008=VECTOR('',#11035,1.);
#3009=VECTOR('',#11036,1.);
#3010=VECTOR('',#11037,1.);
#3011=VECTOR('',#11040,1.);
#3012=VECTOR('',#11041,1.);
#3013=VECTOR('',#11042,1.);
#3014=VECTOR('',#11045,1.);
#3015=VECTOR('',#11046,1.);
#3016=VECTOR('',#11047,1.);
#3017=VECTOR('',#11050,1.);
#3018=VECTOR('',#11051,1.);
#3019=VECTOR('',#11052,1.);
#3020=VECTOR('',#11055,1.);
#3021=VECTOR('',#11056,1.);
#3022=VECTOR('',#11065,1.);
#3023=VECTOR('',#11066,1.);
#3024=VECTOR('',#11067,1.);
#3025=VECTOR('',#11068,1.);
#3026=VECTOR('',#11071,1.);
#3027=VECTOR('',#11072,1.);
#3028=VECTOR('',#11073,1.);
#3029=VECTOR('',#11076,1.);
#3030=VECTOR('',#11077,1.);
#3031=VECTOR('',#11078,1.);
#3032=VECTOR('',#11081,1.);
#3033=VECTOR('',#11082,1.);
#3034=VECTOR('',#11083,1.);
#3035=VECTOR('',#11086,1.);
#3036=VECTOR('',#11087,1.);
#3037=VECTOR('',#11088,1.);
#3038=VECTOR('',#11091,1.);
#3039=VECTOR('',#11092,1.);
#3040=VECTOR('',#11109,0.325);
#3041=VECTOR('',#11114,0.35);
#3042=VECTOR('',#11119,0.335);
#3043=VECTOR('',#11128,0.21);
#3044=VECTOR('',#11131,0.2);
#3045=VECTOR('',#11252,0.6);
#3046=VECTOR('',#11261,0.6);
#3047=VECTOR('',#11270,1.);
#3048=VECTOR('',#11283,0.605);
#3049=VECTOR('',#11290,0.9);
#3050=VECTOR('',#11303,0.605);
#3051=VECTOR('',#11310,0.9);
#3052=VECTOR('',#11321,1.);
#3053=VECTOR('',#11328,0.21);
#3054=VECTOR('',#11333,1.);
#3055=VECTOR('',#11338,0.605);
#3056=VECTOR('',#11345,1.);
#3057=VECTOR('',#11356,1.);
#3058=VECTOR('',#11363,0.21);
#3059=VECTOR('',#11368,1.);
#3060=VECTOR('',#11373,0.605);
#3061=VECTOR('',#11380,1.);
#3062=VECTOR('',#11393,0.605);
#3063=VECTOR('',#11400,0.9);
#3064=VECTOR('',#11413,0.605);
#3065=VECTOR('',#11420,0.9);
#3066=VECTOR('',#11431,1.);
#3067=VECTOR('',#11438,0.21);
#3068=VECTOR('',#11443,1.);
#3069=VECTOR('',#11448,1.005);
#3070=VECTOR('',#11455,1.5);
#3071=VECTOR('',#11466,1.);
#3072=VECTOR('',#11473,0.21);
#3073=VECTOR('',#11478,1.);
#3074=VECTOR('',#11483,1.005);
#3075=VECTOR('',#11490,1.5);
#3076=VECTOR('',#11501,1.);
#3077=VECTOR('',#11508,0.21);
#3078=VECTOR('',#11513,1.);
#3079=VECTOR('',#11518,0.225);
#3080=VECTOR('',#11525,0.225);
#3081=VECTOR('',#11532,0.225);
#3082=VECTOR('',#11539,0.225);
#3083=VECTOR('',#11550,2.3);
#3084=VECTOR('',#11557,0.6);
#3085=VECTOR('',#11564,1.5);
#3086=VECTOR('',#11573,1.);
#3087=VECTOR('',#11574,1.);
#3088=VECTOR('',#11575,1.);
#3089=VECTOR('',#11576,1.);
#3090=VECTOR('',#11579,1.);
#3091=VECTOR('',#11580,1.);
#3092=VECTOR('',#11581,1.);
#3093=VECTOR('',#11584,1.);
#3094=VECTOR('',#11585,1.);
#3095=VECTOR('',#11586,1.);
#3096=VECTOR('',#11589,1.);
#3097=VECTOR('',#11590,1.);
#3098=VECTOR('',#11591,1.);
#3099=VECTOR('',#11594,1.);
#3100=VECTOR('',#11595,1.);
#3101=VECTOR('',#11596,1.);
#3102=VECTOR('',#11599,1.);
#3103=VECTOR('',#11600,1.);
#3104=VECTOR('',#11611,0.235);
#3105=VECTOR('',#11616,0.25);
#3106=VECTOR('',#11621,0.2125);
#3107=CIRCLE('',#8146,0.165);
#3108=CIRCLE('',#8147,0.165);
#3109=CIRCLE('',#8149,0.165);
#3110=CIRCLE('',#8150,0.165);
#3111=CIRCLE('',#8152,0.165);
#3112=CIRCLE('',#8153,0.165);
#3113=CIRCLE('',#8155,0.165);
#3114=CIRCLE('',#8156,0.165);
#3115=CIRCLE('',#8158,0.210000000000001);
#3116=CIRCLE('',#8159,0.210000000000001);
#3117=CIRCLE('',#8161,0.210000000000001);
#3118=CIRCLE('',#8162,0.210000000000001);
#3119=CIRCLE('',#8164,0.210000000000001);
#3120=CIRCLE('',#8165,0.210000000000001);
#3121=CIRCLE('',#8167,0.210000000000001);
#3122=CIRCLE('',#8168,0.210000000000001);
#3123=CIRCLE('',#8170,0.25);
#3124=CIRCLE('',#8171,0.25);
#3125=CIRCLE('',#8173,0.25);
#3126=CIRCLE('',#8174,0.25);
#3127=CIRCLE('',#8176,0.25);
#3128=CIRCLE('',#8177,0.25);
#3129=CIRCLE('',#8179,0.25);
#3130=CIRCLE('',#8180,0.25);
#3131=CIRCLE('',#8189,0.165);
#3132=CIRCLE('',#8190,0.165);
#3133=CIRCLE('',#8192,0.165);
#3134=CIRCLE('',#8193,0.165);
#3135=CIRCLE('',#8195,0.165);
#3136=CIRCLE('',#8196,0.165);
#3137=CIRCLE('',#8198,0.165);
#3138=CIRCLE('',#8199,0.165);
#3139=CIRCLE('',#8201,0.6);
#3140=CIRCLE('',#8203,0.6);
#3141=CIRCLE('',#8207,0.33);
#3142=CIRCLE('',#8209,0.6);
#3143=CIRCLE('',#8210,0.6);
#3144=CIRCLE('',#8212,0.6);
#3145=CIRCLE('',#8215,0.33);
#3146=CIRCLE('',#8217,0.33);
#3147=CIRCLE('',#8219,0.33);
#3148=CIRCLE('',#8226,2.5);
#3149=CIRCLE('',#8227,1.6);
#3150=CIRCLE('',#8229,1.6);
#3151=CIRCLE('',#8231,2.5);
#3152=CIRCLE('',#8235,0.225);
#3153=CIRCLE('',#8236,0.225);
#3154=CIRCLE('',#8238,0.225);
#3155=CIRCLE('',#8239,0.225);
#3156=CIRCLE('',#8241,0.225);
#3157=CIRCLE('',#8242,0.225);
#3158=CIRCLE('',#8244,0.225);
#3159=CIRCLE('',#8245,0.225);
#3160=CIRCLE('',#8247,1.59);
#3161=CIRCLE('',#8248,1.59);
#3162=CIRCLE('',#8250,1.1);
#3163=CIRCLE('',#8252,1.1);
#3164=CIRCLE('',#8254,2.5);
#3165=CIRCLE('',#8255,2.5);
#3166=CIRCLE('',#8260,0.225);
#3167=CIRCLE('',#8261,0.225);
#3168=CIRCLE('',#8263,0.225);
#3169=CIRCLE('',#8264,0.225);
#3170=CIRCLE('',#8266,0.225);
#3171=CIRCLE('',#8267,0.225);
#3172=CIRCLE('',#8269,0.225);
#3173=CIRCLE('',#8270,0.225);
#3174=CIRCLE('',#8272,1.59);
#3175=CIRCLE('',#8273,1.59);
#3176=CIRCLE('',#8275,1.1);
#3177=CIRCLE('',#8277,1.1);
#3178=CIRCLE('',#8279,2.5);
#3179=CIRCLE('',#8280,2.5);
#3180=CIRCLE('',#8285,0.165);
#3181=CIRCLE('',#8286,0.165);
#3182=CIRCLE('',#8288,0.165);
#3183=CIRCLE('',#8289,0.165);
#3184=CIRCLE('',#8291,0.165);
#3185=CIRCLE('',#8292,0.165);
#3186=CIRCLE('',#8294,0.165);
#3187=CIRCLE('',#8295,0.165);
#3188=CIRCLE('',#8297,0.6);
#3189=CIRCLE('',#8299,0.6);
#3190=CIRCLE('',#8303,0.33);
#3191=CIRCLE('',#8305,0.6);
#3192=CIRCLE('',#8306,0.6);
#3193=CIRCLE('',#8308,0.6);
#3194=CIRCLE('',#8311,0.33);
#3195=CIRCLE('',#8313,0.33);
#3196=CIRCLE('',#8315,0.33);
#3197=CIRCLE('',#8322,2.5);
#3198=CIRCLE('',#8323,1.6);
#3199=CIRCLE('',#8325,1.6);
#3200=CIRCLE('',#8327,2.5);
#3201=CIRCLE('',#8331,0.225);
#3202=CIRCLE('',#8332,0.225);
#3203=CIRCLE('',#8334,0.225);
#3204=CIRCLE('',#8335,0.225);
#3205=CIRCLE('',#8337,0.225);
#3206=CIRCLE('',#8338,0.225);
#3207=CIRCLE('',#8340,0.225);
#3208=CIRCLE('',#8341,0.225);
#3209=CIRCLE('',#8343,1.59);
#3210=CIRCLE('',#8344,1.59);
#3211=CIRCLE('',#8346,1.1);
#3212=CIRCLE('',#8348,1.1);
#3213=CIRCLE('',#8350,2.5);
#3214=CIRCLE('',#8351,2.5);
#3215=CIRCLE('',#8356,0.225);
#3216=CIRCLE('',#8357,0.225);
#3217=CIRCLE('',#8359,0.225);
#3218=CIRCLE('',#8360,0.225);
#3219=CIRCLE('',#8362,0.225);
#3220=CIRCLE('',#8363,0.225);
#3221=CIRCLE('',#8365,0.225);
#3222=CIRCLE('',#8366,0.225);
#3223=CIRCLE('',#8368,1.59);
#3224=CIRCLE('',#8369,1.59);
#3225=CIRCLE('',#8371,1.1);
#3226=CIRCLE('',#8373,1.1);
#3227=CIRCLE('',#8375,2.5);
#3228=CIRCLE('',#8376,2.5);
#3229=CIRCLE('',#8381,0.165);
#3230=CIRCLE('',#8382,0.165);
#3231=CIRCLE('',#8384,0.165);
#3232=CIRCLE('',#8385,0.165);
#3233=CIRCLE('',#8387,0.165);
#3234=CIRCLE('',#8388,0.165);
#3235=CIRCLE('',#8390,0.165);
#3236=CIRCLE('',#8391,0.165);
#3237=CIRCLE('',#8394,3.);
#3238=CIRCLE('',#8396,3.);
#3239=CIRCLE('',#8400,2.35);
#3240=CIRCLE('',#8401,2.35);
#3241=CIRCLE('',#8403,3.);
#3242=CIRCLE('',#8404,3.);
#3243=CIRCLE('',#8409,0.225);
#3244=CIRCLE('',#8410,0.225);
#3245=CIRCLE('',#8412,0.225);
#3246=CIRCLE('',#8413,0.225);
#3247=CIRCLE('',#8415,0.225);
#3248=CIRCLE('',#8416,0.225);
#3249=CIRCLE('',#8418,0.225);
#3250=CIRCLE('',#8419,0.225);
#3251=CIRCLE('',#8421,2.34);
#3252=CIRCLE('',#8422,2.34);
#3253=CIRCLE('',#8424,1.9);
#3254=CIRCLE('',#8426,1.9);
#3255=CIRCLE('',#8428,3.);
#3256=CIRCLE('',#8429,3.);
#3257=CIRCLE('',#8434,0.225);
#3258=CIRCLE('',#8435,0.225);
#3259=CIRCLE('',#8437,0.225);
#3260=CIRCLE('',#8438,0.225);
#3261=CIRCLE('',#8440,0.225);
#3262=CIRCLE('',#8441,0.225);
#3263=CIRCLE('',#8443,0.225);
#3264=CIRCLE('',#8444,0.225);
#3265=CIRCLE('',#8446,2.34);
#3266=CIRCLE('',#8447,2.34);
#3267=CIRCLE('',#8449,1.9);
#3268=CIRCLE('',#8451,1.9);
#3269=CIRCLE('',#8453,3.);
#3270=CIRCLE('',#8454,3.);
#3271=CIRCLE('',#8459,0.164999999999999);
#3272=CIRCLE('',#8460,0.164999999999999);
#3273=CIRCLE('',#8463,0.164999999999999);
#3274=CIRCLE('',#8464,0.164999999999999);
#3275=CIRCLE('',#8467,0.5);
#3276=CIRCLE('',#8468,0.5);
#3277=CIRCLE('',#8470,0.275);
#3278=CIRCLE('',#8472,0.5);
#3279=CIRCLE('',#8473,0.5);
#3280=CIRCLE('',#8475,0.275);
#3281=CIRCLE('',#8477,0.5);
#3282=CIRCLE('',#8478,0.5);
#3283=CIRCLE('',#8480,0.275);
#3284=CIRCLE('',#8482,0.5);
#3285=CIRCLE('',#8483,0.5);
#3286=CIRCLE('',#8485,0.275);
#3287=CIRCLE('',#8487,0.275);
#3288=CIRCLE('',#8489,0.275);
#3289=CIRCLE('',#8491,0.275);
#3290=CIRCLE('',#8493,0.275);
#3291=CIRCLE('',#8502,0.225);
#3292=CIRCLE('',#8503,0.225);
#3293=CIRCLE('',#8505,0.225);
#3294=CIRCLE('',#8506,0.225);
#3295=CIRCLE('',#8519,0.4);
#3296=CIRCLE('',#8520,0.4);
#3297=CIRCLE('',#8522,0.225);
#3298=CIRCLE('',#8524,0.225);
#3299=CIRCLE('',#8526,0.9);
#3300=CIRCLE('',#8528,0.9);
#3301=CIRCLE('',#8532,0.4);
#3302=CIRCLE('',#8533,0.4);
#3303=CIRCLE('',#8535,0.225);
#3304=CIRCLE('',#8537,0.225);
#3305=CIRCLE('',#8539,0.9);
#3306=CIRCLE('',#8541,0.9);
#3307=CIRCLE('',#8545,0.4);
#3308=CIRCLE('',#8546,0.4);
#3309=CIRCLE('',#8548,0.225);
#3310=CIRCLE('',#8550,0.225);
#3311=CIRCLE('',#8552,0.9);
#3312=CIRCLE('',#8554,0.9);
#3313=CIRCLE('',#8558,0.4);
#3314=CIRCLE('',#8559,0.4);
#3315=CIRCLE('',#8561,0.225);
#3316=CIRCLE('',#8563,0.225);
#3317=CIRCLE('',#8565,0.9);
#3318=CIRCLE('',#8567,0.9);
#3319=CIRCLE('',#8608,0.2942);
#3320=CIRCLE('',#8610,0.45);
#3321=CIRCLE('',#8612,0.5);
#3322=CIRCLE('',#8614,0.5);
#3323=CIRCLE('',#8616,0.47);
#3324=CIRCLE('',#8618,0.32);
#3325=CIRCLE('',#8620,0.2942);
#3326=CIRCLE('',#8625,1.070235);
#3327=CIRCLE('',#8626,1.070235);
#3328=CIRCLE('',#8627,0.309556);
#3329=CIRCLE('',#8628,1.070235);
#3330=CIRCLE('',#8629,1.070235);
#3331=CIRCLE('',#8631,1.070235);
#3332=CIRCLE('',#8633,0.6);
#3333=CIRCLE('',#8634,0.6);
#3334=CIRCLE('',#8636,0.66);
#3335=CIRCLE('',#8639,1.070235);
#3336=CIRCLE('',#8641,0.66);
#3337=CIRCLE('',#8645,1.129765);
#3338=CIRCLE('',#8646,1.129765);
#3339=CIRCLE('',#8647,0.309556);
#3340=CIRCLE('',#8648,1.129765);
#3341=CIRCLE('',#8649,1.129765);
#3342=CIRCLE('',#8651,1.129765);
#3343=CIRCLE('',#8653,1.54);
#3344=CIRCLE('',#8654,1.129765);
#3345=CIRCLE('',#8656,1.6);
#3346=CIRCLE('',#8658,1.6);
#3347=CIRCLE('',#8660,1.54);
#3348=CIRCLE('',#8665,0.29765);
#3349=CIRCLE('',#8667,0.29765);
#3350=CIRCLE('',#8669,0.29765);
#3351=CIRCLE('',#8671,0.29765);
#3352=CIRCLE('',#8673,0.29765);
#3353=CIRCLE('',#8675,0.29765);
#3354=CIRCLE('',#8677,0.29765);
#3355=CIRCLE('',#8680,0.303778037777585);
#3356=CIRCLE('',#8681,0.303778037777585);
#3357=CIRCLE('',#8683,1.123812);
#3358=CIRCLE('',#8684,1.123812);
#3359=CIRCLE('',#8685,1.123812);
#3360=CIRCLE('',#8686,1.123812);
#3361=CIRCLE('',#8687,1.123812);
#3362=CIRCLE('',#8688,1.123812);
#3363=CIRCLE('',#8689,1.123812);
#3364=CIRCLE('',#8690,1.123812);
#3365=CIRCLE('',#8691,1.123812);
#3366=CIRCLE('',#8693,1.076188);
#3367=CIRCLE('',#8694,0.303778037777585);
#3368=CIRCLE('',#8696,0.303778037777585);
#3369=CIRCLE('',#8698,1.076188);
#3370=CIRCLE('',#8699,0.303778037777585);
#3371=CIRCLE('',#8701,0.303778037777585);
#3372=CIRCLE('',#8703,1.076188);
#3373=CIRCLE('',#8704,1.076188);
#3374=CIRCLE('',#8705,0.303778037777585);
#3375=CIRCLE('',#8707,0.303778037777585);
#3376=CIRCLE('',#8709,1.076188);
#3377=CIRCLE('',#8710,0.303778037777585);
#3378=CIRCLE('',#8712,0.303778037777585);
#3379=CIRCLE('',#8714,1.076188);
#3380=CIRCLE('',#8715,0.303778037777585);
#3381=CIRCLE('',#8717,0.303778037777585);
#3382=CIRCLE('',#8719,1.076188);
#3383=CIRCLE('',#8720,1.076188);
#3384=CIRCLE('',#8721,1.076188);
#3385=CIRCLE('',#8723,0.303778037777585);
#3386=CIRCLE('',#8725,0.303778037777585);
#3387=CIRCLE('',#8730,1.119765);
#3388=CIRCLE('',#8731,1.085235);
#3389=CIRCLE('',#8733,1.119765);
#3390=CIRCLE('',#8735,1.085235);
#3391=CIRCLE('',#8738,1.119765);
#3392=CIRCLE('',#8739,1.085235);
#3393=CIRCLE('',#8741,1.119765);
#3394=CIRCLE('',#8743,1.085235);
#3395=CIRCLE('',#8753,1.63531);
#3396=CIRCLE('',#8754,1.63531);
#3397=CIRCLE('',#8755,0.412776);
#3398=CIRCLE('',#8756,1.63531);
#3399=CIRCLE('',#8757,1.63531);
#3400=CIRCLE('',#8759,1.63531);
#3401=CIRCLE('',#8761,1.);
#3402=CIRCLE('',#8762,1.);
#3403=CIRCLE('',#8764,1.1);
#3404=CIRCLE('',#8767,1.63531);
#3405=CIRCLE('',#8769,1.1);
#3406=CIRCLE('',#8773,1.71469);
#3407=CIRCLE('',#8774,1.71469);
#3408=CIRCLE('',#8775,0.412776);
#3409=CIRCLE('',#8776,1.71469);
#3410=CIRCLE('',#8777,1.71469);
#3411=CIRCLE('',#8779,1.71469);
#3412=CIRCLE('',#8781,2.25);
#3413=CIRCLE('',#8782,1.71469);
#3414=CIRCLE('',#8784,2.35);
#3415=CIRCLE('',#8786,2.35);
#3416=CIRCLE('',#8788,2.25);
#3417=CIRCLE('',#8793,0.3969);
#3418=CIRCLE('',#8795,0.3969);
#3419=CIRCLE('',#8797,0.3969);
#3420=CIRCLE('',#8799,0.3969);
#3421=CIRCLE('',#8801,0.3969);
#3422=CIRCLE('',#8803,0.3969);
#3423=CIRCLE('',#8805,0.3969);
#3424=CIRCLE('',#8807,0.3969);
#3425=CIRCLE('',#8810,0.405071403305639);
#3426=CIRCLE('',#8811,0.405071403305639);
#3427=CIRCLE('',#8813,1.706752);
#3428=CIRCLE('',#8814,1.706752);
#3429=CIRCLE('',#8815,1.706752);
#3430=CIRCLE('',#8816,1.706752);
#3431=CIRCLE('',#8817,1.706752);
#3432=CIRCLE('',#8818,1.706752);
#3433=CIRCLE('',#8819,1.706752);
#3434=CIRCLE('',#8820,1.706752);
#3435=CIRCLE('',#8821,1.706752);
#3436=CIRCLE('',#8823,1.643248);
#3437=CIRCLE('',#8824,0.405071403305639);
#3438=CIRCLE('',#8826,0.405071403305639);
#3439=CIRCLE('',#8828,1.643248);
#3440=CIRCLE('',#8829,0.405071403305639);
#3441=CIRCLE('',#8831,0.405071403305639);
#3442=CIRCLE('',#8833,1.643248);
#3443=CIRCLE('',#8834,0.405071403305639);
#3444=CIRCLE('',#8836,0.405071403305639);
#3445=CIRCLE('',#8838,1.643248);
#3446=CIRCLE('',#8839,0.405071403305639);
#3447=CIRCLE('',#8841,0.405071403305639);
#3448=CIRCLE('',#8843,1.643248);
#3449=CIRCLE('',#8844,0.405071403305639);
#3450=CIRCLE('',#8846,0.405071403305639);
#3451=CIRCLE('',#8848,1.643248);
#3452=CIRCLE('',#8849,0.405071403305639);
#3453=CIRCLE('',#8851,0.405071403305639);
#3454=CIRCLE('',#8853,1.643248);
#3455=CIRCLE('',#8854,1.643248);
#3456=CIRCLE('',#8855,1.643248);
#3457=CIRCLE('',#8857,0.405071403305639);
#3458=CIRCLE('',#8859,0.405071403305639);
#3459=CIRCLE('',#8864,1.70469);
#3460=CIRCLE('',#8865,1.65031);
#3461=CIRCLE('',#8867,1.70469);
#3462=CIRCLE('',#8869,1.65031);
#3463=CIRCLE('',#8872,1.70469);
#3464=CIRCLE('',#8873,1.65031);
#3465=CIRCLE('',#8875,1.70469);
#3466=CIRCLE('',#8877,1.65031);
#3467=CIRCLE('',#8886,0.375);
#3468=CIRCLE('',#8888,0.425);
#3469=CIRCLE('',#8890,0.425);
#3470=CIRCLE('',#8892,0.395);
#3471=CIRCLE('',#8894,0.27);
#3472=CIRCLE('',#8896,0.24505);
#3473=CIRCLE('',#8898,0.24505);
#3474=CIRCLE('',#8900,0.2);
#3475=CIRCLE('',#8920,0.1954);
#3476=CIRCLE('',#8922,0.3);
#3477=CIRCLE('',#8924,0.35);
#3478=CIRCLE('',#8926,0.35);
#3479=CIRCLE('',#8928,0.32);
#3480=CIRCLE('',#8930,0.22);
#3481=CIRCLE('',#8932,0.1954);
#3482=CIRCLE('',#8993,0.6);
#3483=CIRCLE('',#8994,0.6);
#3484=CIRCLE('',#8997,0.6);
#3485=CIRCLE('',#8998,0.6);
#3486=CIRCLE('',#9001,1.);
#3487=CIRCLE('',#9002,1.);
#3488=CIRCLE('',#9007,0.605);
#3489=CIRCLE('',#9008,0.605);
#3490=CIRCLE('',#9010,0.9);
#3491=CIRCLE('',#9011,0.9);
#3492=CIRCLE('',#9016,0.605);
#3493=CIRCLE('',#9017,0.605);
#3494=CIRCLE('',#9019,0.9);
#3495=CIRCLE('',#9020,0.9);
#3496=CIRCLE('',#9025,0.21);
#3497=CIRCLE('',#9027,0.21);
#3498=CIRCLE('',#9028,0.21);
#3499=CIRCLE('',#9031,0.605);
#3500=CIRCLE('',#9032,0.605);
#3501=CIRCLE('',#9034,1.);
#3502=CIRCLE('',#9035,1.);
#3503=CIRCLE('',#9040,0.21);
#3504=CIRCLE('',#9042,0.21);
#3505=CIRCLE('',#9043,0.21);
#3506=CIRCLE('',#9046,0.605);
#3507=CIRCLE('',#9047,0.605);
#3508=CIRCLE('',#9049,1.);
#3509=CIRCLE('',#9050,1.);
#3510=CIRCLE('',#9055,0.605);
#3511=CIRCLE('',#9056,0.605);
#3512=CIRCLE('',#9058,0.9);
#3513=CIRCLE('',#9059,0.9);
#3514=CIRCLE('',#9064,0.605);
#3515=CIRCLE('',#9065,0.605);
#3516=CIRCLE('',#9067,0.9);
#3517=CIRCLE('',#9068,0.9);
#3518=CIRCLE('',#9073,0.21);
#3519=CIRCLE('',#9075,0.21);
#3520=CIRCLE('',#9076,0.21);
#3521=CIRCLE('',#9079,1.005);
#3522=CIRCLE('',#9080,1.005);
#3523=CIRCLE('',#9082,1.5);
#3524=CIRCLE('',#9083,1.5);
#3525=CIRCLE('',#9088,0.21);
#3526=CIRCLE('',#9090,0.21);
#3527=CIRCLE('',#9091,0.21);
#3528=CIRCLE('',#9094,1.005);
#3529=CIRCLE('',#9095,1.005);
#3530=CIRCLE('',#9097,1.5);
#3531=CIRCLE('',#9098,1.5);
#3532=CIRCLE('',#9103,0.21);
#3533=CIRCLE('',#9105,0.21);
#3534=CIRCLE('',#9106,0.21);
#3535=CIRCLE('',#9109,0.225);
#3536=CIRCLE('',#9110,0.225);
#3537=CIRCLE('',#9112,0.225);
#3538=CIRCLE('',#9113,0.225);
#3539=CIRCLE('',#9115,0.225);
#3540=CIRCLE('',#9116,0.225);
#3541=CIRCLE('',#9118,0.225);
#3542=CIRCLE('',#9119,0.225);
#3543=CIRCLE('',#9121,2.3);
#3544=CIRCLE('',#9122,1.5);
#3545=CIRCLE('',#9124,2.3);
#3546=CIRCLE('',#9126,0.6);
#3547=CIRCLE('',#9127,0.6);
#3548=CIRCLE('',#9129,1.5);
#3549=CIRCLE('',#9141,0.22);
#3550=CIRCLE('',#9143,0.24505);
#3551=CIRCLE('',#9145,0.24505);
#3552=CIRCLE('',#9147,0.175);
#3553=VERTEX_POINT('',#11662);
#3554=VERTEX_POINT('',#11664);
#3555=VERTEX_POINT('',#11668);
#3556=VERTEX_POINT('',#11670);
#3557=VERTEX_POINT('',#11674);
#3558=VERTEX_POINT('',#11676);
#3559=VERTEX_POINT('',#11680);
#3560=VERTEX_POINT('',#11682);
#3561=VERTEX_POINT('',#11686);
#3562=VERTEX_POINT('',#11688);
#3563=VERTEX_POINT('',#11692);
#3564=VERTEX_POINT('',#11694);
#3565=VERTEX_POINT('',#11698);
#3566=VERTEX_POINT('',#11700);
#3567=VERTEX_POINT('',#11704);
#3568=VERTEX_POINT('',#11706);
#3569=VERTEX_POINT('',#11710);
#3570=VERTEX_POINT('',#11712);
#3571=VERTEX_POINT('',#11716);
#3572=VERTEX_POINT('',#11718);
#3573=VERTEX_POINT('',#11722);
#3574=VERTEX_POINT('',#11724);
#3575=VERTEX_POINT('',#11728);
#3576=VERTEX_POINT('',#11730);
#3577=VERTEX_POINT('',#11734);
#3578=VERTEX_POINT('',#11735);
#3579=VERTEX_POINT('',#11737);
#3580=VERTEX_POINT('',#11739);
#3581=VERTEX_POINT('',#11743);
#3582=VERTEX_POINT('',#11745);
#3583=VERTEX_POINT('',#11749);
#3584=VERTEX_POINT('',#11751);
#3585=VERTEX_POINT('',#11761);
#3586=VERTEX_POINT('',#11763);
#3587=VERTEX_POINT('',#11767);
#3588=VERTEX_POINT('',#11769);
#3589=VERTEX_POINT('',#11773);
#3590=VERTEX_POINT('',#11775);
#3591=VERTEX_POINT('',#11779);
#3592=VERTEX_POINT('',#11781);
#3593=VERTEX_POINT('',#11785);
#3594=VERTEX_POINT('',#11786);
#3595=VERTEX_POINT('',#11790);
#3596=VERTEX_POINT('',#11792);
#3597=VERTEX_POINT('',#11797);
#3598=VERTEX_POINT('',#11800);
#3599=VERTEX_POINT('',#11801);
#3600=VERTEX_POINT('',#11803);
#3601=VERTEX_POINT('',#11807);
#3602=VERTEX_POINT('',#11812);
#3603=VERTEX_POINT('',#11815);
#3604=VERTEX_POINT('',#11819);
#3605=VERTEX_POINT('',#11823);
#3606=VERTEX_POINT('',#11824);
#3607=VERTEX_POINT('',#11826);
#3608=VERTEX_POINT('',#11828);
#3609=VERTEX_POINT('',#11832);
#3610=VERTEX_POINT('',#11833);
#3611=VERTEX_POINT('',#11835);
#3612=VERTEX_POINT('',#11837);
#3613=VERTEX_POINT('',#11841);
#3614=VERTEX_POINT('',#11843);
#3615=VERTEX_POINT('',#11847);
#3616=VERTEX_POINT('',#11849);
#3617=VERTEX_POINT('',#11857);
#3618=VERTEX_POINT('',#11860);
#3619=VERTEX_POINT('',#11868);
#3620=VERTEX_POINT('',#11870);
#3621=VERTEX_POINT('',#11874);
#3622=VERTEX_POINT('',#11876);
#3623=VERTEX_POINT('',#11880);
#3624=VERTEX_POINT('',#11882);
#3625=VERTEX_POINT('',#11886);
#3626=VERTEX_POINT('',#11888);
#3627=VERTEX_POINT('',#11892);
#3628=VERTEX_POINT('',#11894);
#3629=VERTEX_POINT('',#11898);
#3630=VERTEX_POINT('',#11901);
#3631=VERTEX_POINT('',#11905);
#3632=VERTEX_POINT('',#11907);
#3633=VERTEX_POINT('',#11914);
#3634=VERTEX_POINT('',#11916);
#3635=VERTEX_POINT('',#11920);
#3636=VERTEX_POINT('',#11922);
#3637=VERTEX_POINT('',#11926);
#3638=VERTEX_POINT('',#11928);
#3639=VERTEX_POINT('',#11932);
#3640=VERTEX_POINT('',#11934);
#3641=VERTEX_POINT('',#11938);
#3642=VERTEX_POINT('',#11940);
#3643=VERTEX_POINT('',#11944);
#3644=VERTEX_POINT('',#11947);
#3645=VERTEX_POINT('',#11951);
#3646=VERTEX_POINT('',#11953);
#3647=VERTEX_POINT('',#11960);
#3648=VERTEX_POINT('',#11962);
#3649=VERTEX_POINT('',#11966);
#3650=VERTEX_POINT('',#11968);
#3651=VERTEX_POINT('',#11972);
#3652=VERTEX_POINT('',#11974);
#3653=VERTEX_POINT('',#11978);
#3654=VERTEX_POINT('',#11980);
#3655=VERTEX_POINT('',#11984);
#3656=VERTEX_POINT('',#11985);
#3657=VERTEX_POINT('',#11989);
#3658=VERTEX_POINT('',#11991);
#3659=VERTEX_POINT('',#11996);
#3660=VERTEX_POINT('',#11999);
#3661=VERTEX_POINT('',#12000);
#3662=VERTEX_POINT('',#12002);
#3663=VERTEX_POINT('',#12006);
#3664=VERTEX_POINT('',#12011);
#3665=VERTEX_POINT('',#12014);
#3666=VERTEX_POINT('',#12018);
#3667=VERTEX_POINT('',#12022);
#3668=VERTEX_POINT('',#12023);
#3669=VERTEX_POINT('',#12025);
#3670=VERTEX_POINT('',#12027);
#3671=VERTEX_POINT('',#12031);
#3672=VERTEX_POINT('',#12032);
#3673=VERTEX_POINT('',#12034);
#3674=VERTEX_POINT('',#12036);
#3675=VERTEX_POINT('',#12040);
#3676=VERTEX_POINT('',#12042);
#3677=VERTEX_POINT('',#12046);
#3678=VERTEX_POINT('',#12048);
#3679=VERTEX_POINT('',#12056);
#3680=VERTEX_POINT('',#12059);
#3681=VERTEX_POINT('',#12067);
#3682=VERTEX_POINT('',#12069);
#3683=VERTEX_POINT('',#12073);
#3684=VERTEX_POINT('',#12075);
#3685=VERTEX_POINT('',#12079);
#3686=VERTEX_POINT('',#12081);
#3687=VERTEX_POINT('',#12085);
#3688=VERTEX_POINT('',#12087);
#3689=VERTEX_POINT('',#12091);
#3690=VERTEX_POINT('',#12093);
#3691=VERTEX_POINT('',#12097);
#3692=VERTEX_POINT('',#12100);
#3693=VERTEX_POINT('',#12104);
#3694=VERTEX_POINT('',#12106);
#3695=VERTEX_POINT('',#12113);
#3696=VERTEX_POINT('',#12115);
#3697=VERTEX_POINT('',#12119);
#3698=VERTEX_POINT('',#12121);
#3699=VERTEX_POINT('',#12125);
#3700=VERTEX_POINT('',#12127);
#3701=VERTEX_POINT('',#12131);
#3702=VERTEX_POINT('',#12133);
#3703=VERTEX_POINT('',#12137);
#3704=VERTEX_POINT('',#12139);
#3705=VERTEX_POINT('',#12143);
#3706=VERTEX_POINT('',#12146);
#3707=VERTEX_POINT('',#12150);
#3708=VERTEX_POINT('',#12152);
#3709=VERTEX_POINT('',#12159);
#3710=VERTEX_POINT('',#12161);
#3711=VERTEX_POINT('',#12165);
#3712=VERTEX_POINT('',#12167);
#3713=VERTEX_POINT('',#12171);
#3714=VERTEX_POINT('',#12173);
#3715=VERTEX_POINT('',#12177);
#3716=VERTEX_POINT('',#12179);
#3717=VERTEX_POINT('',#12183);
#3718=VERTEX_POINT('',#12184);
#3719=VERTEX_POINT('',#12186);
#3720=VERTEX_POINT('',#12188);
#3721=VERTEX_POINT('',#12192);
#3722=VERTEX_POINT('',#12194);
#3723=VERTEX_POINT('',#12198);
#3724=VERTEX_POINT('',#12200);
#3725=VERTEX_POINT('',#12208);
#3726=VERTEX_POINT('',#12210);
#3727=VERTEX_POINT('',#12214);
#3728=VERTEX_POINT('',#12216);
#3729=VERTEX_POINT('',#12223);
#3730=VERTEX_POINT('',#12225);
#3731=VERTEX_POINT('',#12229);
#3732=VERTEX_POINT('',#12231);
#3733=VERTEX_POINT('',#12235);
#3734=VERTEX_POINT('',#12237);
#3735=VERTEX_POINT('',#12241);
#3736=VERTEX_POINT('',#12243);
#3737=VERTEX_POINT('',#12247);
#3738=VERTEX_POINT('',#12249);
#3739=VERTEX_POINT('',#12253);
#3740=VERTEX_POINT('',#12256);
#3741=VERTEX_POINT('',#12260);
#3742=VERTEX_POINT('',#12262);
#3743=VERTEX_POINT('',#12269);
#3744=VERTEX_POINT('',#12271);
#3745=VERTEX_POINT('',#12275);
#3746=VERTEX_POINT('',#12277);
#3747=VERTEX_POINT('',#12281);
#3748=VERTEX_POINT('',#12283);
#3749=VERTEX_POINT('',#12287);
#3750=VERTEX_POINT('',#12289);
#3751=VERTEX_POINT('',#12293);
#3752=VERTEX_POINT('',#12295);
#3753=VERTEX_POINT('',#12299);
#3754=VERTEX_POINT('',#12302);
#3755=VERTEX_POINT('',#12306);
#3756=VERTEX_POINT('',#12308);
#3757=VERTEX_POINT('',#12315);
#3758=VERTEX_POINT('',#12317);
#3759=VERTEX_POINT('',#12322);
#3760=VERTEX_POINT('',#12324);
#3761=VERTEX_POINT('',#12329);
#3762=VERTEX_POINT('',#12331);
#3763=VERTEX_POINT('',#12335);
#3764=VERTEX_POINT('',#12338);
#3765=VERTEX_POINT('',#12340);
#3766=VERTEX_POINT('',#12344);
#3767=VERTEX_POINT('',#12347);
#3768=VERTEX_POINT('',#12349);
#3769=VERTEX_POINT('',#12353);
#3770=VERTEX_POINT('',#12356);
#3771=VERTEX_POINT('',#12358);
#3772=VERTEX_POINT('',#12362);
#3773=VERTEX_POINT('',#12365);
#3774=VERTEX_POINT('',#12369);
#3775=VERTEX_POINT('',#12373);
#3776=VERTEX_POINT('',#12377);
#3777=VERTEX_POINT('',#12381);
#3778=VERTEX_POINT('',#12382);
#3779=VERTEX_POINT('',#12384);
#3780=VERTEX_POINT('',#12386);
#3781=VERTEX_POINT('',#12390);
#3782=VERTEX_POINT('',#12392);
#3783=VERTEX_POINT('',#12396);
#3784=VERTEX_POINT('',#12398);
#3785=VERTEX_POINT('',#12408);
#3786=VERTEX_POINT('',#12410);
#3787=VERTEX_POINT('',#12414);
#3788=VERTEX_POINT('',#12416);
#3789=VERTEX_POINT('',#12420);
#3790=VERTEX_POINT('',#12421);
#3791=VERTEX_POINT('',#12423);
#3792=VERTEX_POINT('',#12425);
#3793=VERTEX_POINT('',#12429);
#3794=VERTEX_POINT('',#12431);
#3795=VERTEX_POINT('',#12435);
#3796=VERTEX_POINT('',#12437);
#3797=VERTEX_POINT('',#12441);
#3798=VERTEX_POINT('',#12442);
#3799=VERTEX_POINT('',#12444);
#3800=VERTEX_POINT('',#12446);
#3801=VERTEX_POINT('',#12450);
#3802=VERTEX_POINT('',#12452);
#3803=VERTEX_POINT('',#12457);
#3804=VERTEX_POINT('',#12461);
#3805=VERTEX_POINT('',#12471);
#3806=VERTEX_POINT('',#12473);
#3807=VERTEX_POINT('',#12477);
#3808=VERTEX_POINT('',#12480);
#3809=VERTEX_POINT('',#12484);
#3810=VERTEX_POINT('',#12486);
#3811=VERTEX_POINT('',#12487);
#3812=VERTEX_POINT('',#12489);
#3813=VERTEX_POINT('',#12491);
#3814=VERTEX_POINT('',#12495);
#3815=VERTEX_POINT('',#12499);
#3816=VERTEX_POINT('',#12501);
#3817=VERTEX_POINT('',#12503);
#3818=VERTEX_POINT('',#12505);
#3819=VERTEX_POINT('',#12507);
#3820=VERTEX_POINT('',#12509);
#3821=VERTEX_POINT('',#12513);
#3822=VERTEX_POINT('',#12515);
#3823=VERTEX_POINT('',#12517);
#3824=VERTEX_POINT('',#12519);
#3825=VERTEX_POINT('',#12521);
#3826=VERTEX_POINT('',#12525);
#3827=VERTEX_POINT('',#12527);
#3828=VERTEX_POINT('',#12531);
#3829=VERTEX_POINT('',#12534);
#3830=VERTEX_POINT('',#12538);
#3831=VERTEX_POINT('',#12540);
#3832=VERTEX_POINT('',#12542);
#3833=VERTEX_POINT('',#12546);
#3834=VERTEX_POINT('',#12550);
#3835=VERTEX_POINT('',#12554);
#3836=VERTEX_POINT('',#12558);
#3837=VERTEX_POINT('',#12560);
#3838=VERTEX_POINT('',#12564);
#3839=VERTEX_POINT('',#12567);
#3840=VERTEX_POINT('',#12571);
#3841=VERTEX_POINT('',#12573);
#3842=VERTEX_POINT('',#12575);
#3843=VERTEX_POINT('',#12579);
#3844=VERTEX_POINT('',#12583);
#3845=VERTEX_POINT('',#12585);
#3846=VERTEX_POINT('',#12591);
#3847=VERTEX_POINT('',#12593);
#3848=VERTEX_POINT('',#12597);
#3849=VERTEX_POINT('',#12600);
#3850=VERTEX_POINT('',#12604);
#3851=VERTEX_POINT('',#12606);
#3852=VERTEX_POINT('',#12607);
#3853=VERTEX_POINT('',#12609);
#3854=VERTEX_POINT('',#12611);
#3855=VERTEX_POINT('',#12615);
#3856=VERTEX_POINT('',#12619);
#3857=VERTEX_POINT('',#12622);
#3858=VERTEX_POINT('',#12626);
#3859=VERTEX_POINT('',#12630);
#3860=VERTEX_POINT('',#12631);
#3861=VERTEX_POINT('',#12633);
#3862=VERTEX_POINT('',#12635);
#3863=VERTEX_POINT('',#12639);
#3864=VERTEX_POINT('',#12641);
#3865=VERTEX_POINT('',#12645);
#3866=VERTEX_POINT('',#12647);
#3867=VERTEX_POINT('',#12654);
#3868=VERTEX_POINT('',#12661);
#3869=VERTEX_POINT('',#12674);
#3870=VERTEX_POINT('',#12675);
#3871=VERTEX_POINT('',#12677);
#3872=VERTEX_POINT('',#12679);
#3873=VERTEX_POINT('',#12683);
#3874=VERTEX_POINT('',#12685);
#3875=VERTEX_POINT('',#12689);
#3876=VERTEX_POINT('',#12691);
#3877=VERTEX_POINT('',#12701);
#3878=VERTEX_POINT('',#12702);
#3879=VERTEX_POINT('',#12704);
#3880=VERTEX_POINT('',#12706);
#3881=VERTEX_POINT('',#12710);
#3882=VERTEX_POINT('',#12712);
#3883=VERTEX_POINT('',#12716);
#3884=VERTEX_POINT('',#12718);
#3885=VERTEX_POINT('',#12728);
#3886=VERTEX_POINT('',#12729);
#3887=VERTEX_POINT('',#12731);
#3888=VERTEX_POINT('',#12733);
#3889=VERTEX_POINT('',#12737);
#3890=VERTEX_POINT('',#12739);
#3891=VERTEX_POINT('',#12743);
#3892=VERTEX_POINT('',#12745);
#3893=VERTEX_POINT('',#12749);
#3894=VERTEX_POINT('',#12751);
#3895=VERTEX_POINT('',#12755);
#3896=VERTEX_POINT('',#12757);
#3897=VERTEX_POINT('',#12766);
#3898=VERTEX_POINT('',#12769);
#3899=VERTEX_POINT('',#12772);
#3900=VERTEX_POINT('',#12776);
#3901=VERTEX_POINT('',#12780);
#3902=VERTEX_POINT('',#12784);
#3903=VERTEX_POINT('',#12787);
#3904=VERTEX_POINT('',#12795);
#3905=VERTEX_POINT('',#12796);
#3906=VERTEX_POINT('',#12799);
#3907=VERTEX_POINT('',#12801);
#3908=VERTEX_POINT('',#12805);
#3909=VERTEX_POINT('',#12809);
#3910=VERTEX_POINT('',#12811);
#3911=VERTEX_POINT('',#12815);
#3912=VERTEX_POINT('',#12820);
#3913=VERTEX_POINT('',#12824);
#3914=VERTEX_POINT('',#12830);
#3915=VERTEX_POINT('',#12831);
#3916=VERTEX_POINT('',#12834);
#3917=VERTEX_POINT('',#12836);
#3918=VERTEX_POINT('',#12840);
#3919=VERTEX_POINT('',#12844);
#3920=VERTEX_POINT('',#12846);
#3921=VERTEX_POINT('',#12849);
#3922=VERTEX_POINT('',#12853);
#3923=VERTEX_POINT('',#12857);
#3924=VERTEX_POINT('',#12865);
#3925=VERTEX_POINT('',#12866);
#3926=VERTEX_POINT('',#12869);
#3927=VERTEX_POINT('',#12870);
#3928=VERTEX_POINT('',#12873);
#3929=VERTEX_POINT('',#12874);
#3930=VERTEX_POINT('',#12877);
#3931=VERTEX_POINT('',#12878);
#3932=VERTEX_POINT('',#12881);
#3933=VERTEX_POINT('',#12882);
#3934=VERTEX_POINT('',#12885);
#3935=VERTEX_POINT('',#12886);
#3936=VERTEX_POINT('',#12889);
#3937=VERTEX_POINT('',#12890);
#3938=VERTEX_POINT('',#12894);
#3939=VERTEX_POINT('',#12895);
#3940=VERTEX_POINT('',#12918);
#3941=VERTEX_POINT('',#12920);
#3942=VERTEX_POINT('',#12945);
#3943=VERTEX_POINT('',#12947);
#3944=VERTEX_POINT('',#12970);
#3945=VERTEX_POINT('',#12972);
#3946=VERTEX_POINT('',#12995);
#3947=VERTEX_POINT('',#12997);
#3948=VERTEX_POINT('',#13000);
#3949=VERTEX_POINT('',#13002);
#3950=VERTEX_POINT('',#13025);
#3951=VERTEX_POINT('',#13027);
#3952=VERTEX_POINT('',#13050);
#3953=VERTEX_POINT('',#13052);
#3954=VERTEX_POINT('',#13075);
#3955=VERTEX_POINT('',#13077);
#3956=VERTEX_POINT('',#13102);
#3957=VERTEX_POINT('',#13106);
#3958=VERTEX_POINT('',#13131);
#3959=VERTEX_POINT('',#13135);
#3960=VERTEX_POINT('',#13160);
#3961=VERTEX_POINT('',#13162);
#3962=VERTEX_POINT('',#13166);
#3963=VERTEX_POINT('',#13191);
#3964=VERTEX_POINT('',#13195);
#3965=VERTEX_POINT('',#13220);
#3966=VERTEX_POINT('',#13224);
#3967=VERTEX_POINT('',#13249);
#3968=VERTEX_POINT('',#13252);
#3969=VERTEX_POINT('',#13254);
#3970=VERTEX_POINT('',#13286);
#3971=VERTEX_POINT('',#13288);
#3972=VERTEX_POINT('',#13291);
#3973=VERTEX_POINT('',#13295);
#3974=VERTEX_POINT('',#13300);
#3975=VERTEX_POINT('',#13302);
#3976=VERTEX_POINT('',#13305);
#3977=VERTEX_POINT('',#13309);
#3978=VERTEX_POINT('',#13321);
#3979=VERTEX_POINT('',#13322);
#3980=VERTEX_POINT('',#13325);
#3981=VERTEX_POINT('',#13327);
#3982=VERTEX_POINT('',#13331);
#3983=VERTEX_POINT('',#13335);
#3984=VERTEX_POINT('',#13337);
#3985=VERTEX_POINT('',#13341);
#3986=VERTEX_POINT('',#13346);
#3987=VERTEX_POINT('',#13350);
#3988=VERTEX_POINT('',#13356);
#3989=VERTEX_POINT('',#13357);
#3990=VERTEX_POINT('',#13360);
#3991=VERTEX_POINT('',#13362);
#3992=VERTEX_POINT('',#13366);
#3993=VERTEX_POINT('',#13370);
#3994=VERTEX_POINT('',#13372);
#3995=VERTEX_POINT('',#13375);
#3996=VERTEX_POINT('',#13379);
#3997=VERTEX_POINT('',#13383);
#3998=VERTEX_POINT('',#13391);
#3999=VERTEX_POINT('',#13392);
#4000=VERTEX_POINT('',#13395);
#4001=VERTEX_POINT('',#13396);
#4002=VERTEX_POINT('',#13399);
#4003=VERTEX_POINT('',#13400);
#4004=VERTEX_POINT('',#13403);
#4005=VERTEX_POINT('',#13404);
#4006=VERTEX_POINT('',#13407);
#4007=VERTEX_POINT('',#13408);
#4008=VERTEX_POINT('',#13411);
#4009=VERTEX_POINT('',#13412);
#4010=VERTEX_POINT('',#13415);
#4011=VERTEX_POINT('',#13416);
#4012=VERTEX_POINT('',#13419);
#4013=VERTEX_POINT('',#13420);
#4014=VERTEX_POINT('',#13424);
#4015=VERTEX_POINT('',#13425);
#4016=VERTEX_POINT('',#13448);
#4017=VERTEX_POINT('',#13450);
#4018=VERTEX_POINT('',#13475);
#4019=VERTEX_POINT('',#13477);
#4020=VERTEX_POINT('',#13500);
#4021=VERTEX_POINT('',#13502);
#4022=VERTEX_POINT('',#13525);
#4023=VERTEX_POINT('',#13527);
#4024=VERTEX_POINT('',#13540);
#4025=VERTEX_POINT('',#13543);
#4026=VERTEX_POINT('',#13556);
#4027=VERTEX_POINT('',#13558);
#4028=VERTEX_POINT('',#13581);
#4029=VERTEX_POINT('',#13583);
#4030=VERTEX_POINT('',#13606);
#4031=VERTEX_POINT('',#13608);
#4032=VERTEX_POINT('',#13631);
#4033=VERTEX_POINT('',#13633);
#4034=VERTEX_POINT('',#13658);
#4035=VERTEX_POINT('',#13662);
#4036=VERTEX_POINT('',#13687);
#4037=VERTEX_POINT('',#13691);
#4038=VERTEX_POINT('',#13716);
#4039=VERTEX_POINT('',#13720);
#4040=VERTEX_POINT('',#13721);
#4041=VERTEX_POINT('',#13748);
#4042=VERTEX_POINT('',#13752);
#4043=VERTEX_POINT('',#13777);
#4044=VERTEX_POINT('',#13781);
#4045=VERTEX_POINT('',#13806);
#4046=VERTEX_POINT('',#13810);
#4047=VERTEX_POINT('',#13835);
#4048=VERTEX_POINT('',#13838);
#4049=VERTEX_POINT('',#13840);
#4050=VERTEX_POINT('',#13872);
#4051=VERTEX_POINT('',#13874);
#4052=VERTEX_POINT('',#13877);
#4053=VERTEX_POINT('',#13881);
#4054=VERTEX_POINT('',#13886);
#4055=VERTEX_POINT('',#13888);
#4056=VERTEX_POINT('',#13891);
#4057=VERTEX_POINT('',#13895);
#4058=VERTEX_POINT('',#13906);
#4059=VERTEX_POINT('',#13909);
#4060=VERTEX_POINT('',#13913);
#4061=VERTEX_POINT('',#13917);
#4062=VERTEX_POINT('',#13921);
#4063=VERTEX_POINT('',#13924);
#4064=VERTEX_POINT('',#13928);
#4065=VERTEX_POINT('',#13932);
#4066=VERTEX_POINT('',#13937);
#4067=VERTEX_POINT('',#13938);
#4068=VERTEX_POINT('',#13940);
#4069=VERTEX_POINT('',#13942);
#4070=VERTEX_POINT('',#13946);
#4071=VERTEX_POINT('',#13948);
#4072=VERTEX_POINT('',#13952);
#4073=VERTEX_POINT('',#13954);
#4074=VERTEX_POINT('',#13958);
#4075=VERTEX_POINT('',#13960);
#4076=VERTEX_POINT('',#13964);
#4077=VERTEX_POINT('',#13966);
#4078=VERTEX_POINT('',#13976);
#4079=VERTEX_POINT('',#13977);
#4080=VERTEX_POINT('',#13979);
#4081=VERTEX_POINT('',#13981);
#4082=VERTEX_POINT('',#13985);
#4083=VERTEX_POINT('',#13987);
#4084=VERTEX_POINT('',#13991);
#4085=VERTEX_POINT('',#13993);
#4086=VERTEX_POINT('',#13997);
#4087=VERTEX_POINT('',#13999);
#4088=VERTEX_POINT('',#14003);
#4089=VERTEX_POINT('',#14005);
#4090=VERTEX_POINT('',#14014);
#4091=VERTEX_POINT('',#14017);
#4092=VERTEX_POINT('',#14020);
#4093=VERTEX_POINT('',#14024);
#4094=VERTEX_POINT('',#14028);
#4095=VERTEX_POINT('',#14032);
#4096=VERTEX_POINT('',#14035);
#4097=VERTEX_POINT('',#14099);
#4098=VERTEX_POINT('',#14101);
#4099=VERTEX_POINT('',#14106);
#4100=VERTEX_POINT('',#14108);
#4101=VERTEX_POINT('',#14113);
#4102=VERTEX_POINT('',#14115);
#4103=VERTEX_POINT('',#14122);
#4104=VERTEX_POINT('',#14124);
#4105=VERTEX_POINT('',#14128);
#4106=VERTEX_POINT('',#14130);
#4107=VERTEX_POINT('',#14137);
#4108=VERTEX_POINT('',#14139);
#4109=VERTEX_POINT('',#14143);
#4110=VERTEX_POINT('',#14145);
#4111=VERTEX_POINT('',#14152);
#4112=VERTEX_POINT('',#14153);
#4113=VERTEX_POINT('',#14157);
#4114=VERTEX_POINT('',#14168);
#4115=VERTEX_POINT('',#14170);
#4116=VERTEX_POINT('',#14172);
#4117=VERTEX_POINT('',#14209);
#4118=VERTEX_POINT('',#14224);
#4119=VERTEX_POINT('',#14226);
#4120=VERTEX_POINT('',#14230);
#4121=VERTEX_POINT('',#14232);
#4122=VERTEX_POINT('',#14239);
#4123=VERTEX_POINT('',#14240);
#4124=VERTEX_POINT('',#14244);
#4125=VERTEX_POINT('',#14255);
#4126=VERTEX_POINT('',#14257);
#4127=VERTEX_POINT('',#14259);
#4128=VERTEX_POINT('',#14296);
#4129=VERTEX_POINT('',#14311);
#4130=VERTEX_POINT('',#14313);
#4131=VERTEX_POINT('',#14317);
#4132=VERTEX_POINT('',#14319);
#4133=VERTEX_POINT('',#14326);
#4134=VERTEX_POINT('',#14328);
#4135=VERTEX_POINT('',#14332);
#4136=VERTEX_POINT('',#14334);
#4137=VERTEX_POINT('',#14341);
#4138=VERTEX_POINT('',#14343);
#4139=VERTEX_POINT('',#14347);
#4140=VERTEX_POINT('',#14349);
#4141=VERTEX_POINT('',#14356);
#4142=VERTEX_POINT('',#14357);
#4143=VERTEX_POINT('',#14361);
#4144=VERTEX_POINT('',#14376);
#4145=VERTEX_POINT('',#14378);
#4146=VERTEX_POINT('',#14380);
#4147=VERTEX_POINT('',#14417);
#4148=VERTEX_POINT('',#14436);
#4149=VERTEX_POINT('',#14438);
#4150=VERTEX_POINT('',#14442);
#4151=VERTEX_POINT('',#14444);
#4152=VERTEX_POINT('',#14451);
#4153=VERTEX_POINT('',#14452);
#4154=VERTEX_POINT('',#14456);
#4155=VERTEX_POINT('',#14471);
#4156=VERTEX_POINT('',#14473);
#4157=VERTEX_POINT('',#14475);
#4158=VERTEX_POINT('',#14512);
#4159=VERTEX_POINT('',#14531);
#4160=VERTEX_POINT('',#14533);
#4161=VERTEX_POINT('',#14537);
#4162=VERTEX_POINT('',#14539);
#4163=VERTEX_POINT('',#14546);
#4164=VERTEX_POINT('',#14547);
#4165=VERTEX_POINT('',#14551);
#4166=VERTEX_POINT('',#14562);
#4167=VERTEX_POINT('',#14564);
#4168=VERTEX_POINT('',#14566);
#4169=VERTEX_POINT('',#14603);
#4170=VERTEX_POINT('',#14618);
#4171=VERTEX_POINT('',#14620);
#4172=VERTEX_POINT('',#14624);
#4173=VERTEX_POINT('',#14626);
#4174=VERTEX_POINT('',#14630);
#4175=VERTEX_POINT('',#14632);
#4176=VERTEX_POINT('',#14636);
#4177=VERTEX_POINT('',#14638);
#4178=VERTEX_POINT('',#14642);
#4179=VERTEX_POINT('',#14644);
#4180=VERTEX_POINT('',#14647);
#4181=VERTEX_POINT('',#14651);
#4182=VERTEX_POINT('',#14653);
#4183=VERTEX_POINT('',#14657);
#4184=VERTEX_POINT('',#14664);
#4185=VERTEX_POINT('',#14665);
#4186=VERTEX_POINT('',#14667);
#4187=VERTEX_POINT('',#14669);
#4188=VERTEX_POINT('',#14673);
#4189=VERTEX_POINT('',#14675);
#4190=VERTEX_POINT('',#14679);
#4191=VERTEX_POINT('',#14681);
#4192=VERTEX_POINT('',#14685);
#4193=VERTEX_POINT('',#14687);
#4194=VERTEX_POINT('',#14691);
#4195=VERTEX_POINT('',#14693);
#4196=VERTEX_POINT('',#14701);
#4197=VERTEX_POINT('',#14704);
#4198=VERTEX_POINT('',#14708);
#4199=VERTEX_POINT('',#14712);
#4200=EDGE_CURVE('',#3553,#3553,#3107,.T.);
#4201=EDGE_CURVE('',#3553,#3554,#2219,.T.);
#4202=EDGE_CURVE('',#3554,#3554,#3108,.T.);
#4203=EDGE_CURVE('',#3555,#3555,#3109,.T.);
#4204=EDGE_CURVE('',#3555,#3556,#2220,.T.);
#4205=EDGE_CURVE('',#3556,#3556,#3110,.T.);
#4206=EDGE_CURVE('',#3557,#3557,#3111,.T.);
#4207=EDGE_CURVE('',#3557,#3558,#2221,.T.);
#4208=EDGE_CURVE('',#3558,#3558,#3112,.T.);
#4209=EDGE_CURVE('',#3559,#3559,#3113,.T.);
#4210=EDGE_CURVE('',#3559,#3560,#2222,.T.);
#4211=EDGE_CURVE('',#3560,#3560,#3114,.T.);
#4212=EDGE_CURVE('',#3561,#3561,#3115,.T.);
#4213=EDGE_CURVE('',#3561,#3562,#2223,.T.);
#4214=EDGE_CURVE('',#3562,#3562,#3116,.T.);
#4215=EDGE_CURVE('',#3563,#3563,#3117,.T.);
#4216=EDGE_CURVE('',#3563,#3564,#2224,.T.);
#4217=EDGE_CURVE('',#3564,#3564,#3118,.T.);
#4218=EDGE_CURVE('',#3565,#3565,#3119,.T.);
#4219=EDGE_CURVE('',#3565,#3566,#2225,.T.);
#4220=EDGE_CURVE('',#3566,#3566,#3120,.T.);
#4221=EDGE_CURVE('',#3567,#3567,#3121,.T.);
#4222=EDGE_CURVE('',#3567,#3568,#2226,.T.);
#4223=EDGE_CURVE('',#3568,#3568,#3122,.T.);
#4224=EDGE_CURVE('',#3569,#3569,#3123,.T.);
#4225=EDGE_CURVE('',#3569,#3570,#2227,.T.);
#4226=EDGE_CURVE('',#3570,#3570,#3124,.T.);
#4227=EDGE_CURVE('',#3571,#3571,#3125,.T.);
#4228=EDGE_CURVE('',#3571,#3572,#2228,.T.);
#4229=EDGE_CURVE('',#3572,#3572,#3126,.T.);
#4230=EDGE_CURVE('',#3573,#3573,#3127,.T.);
#4231=EDGE_CURVE('',#3573,#3574,#2229,.T.);
#4232=EDGE_CURVE('',#3574,#3574,#3128,.T.);
#4233=EDGE_CURVE('',#3575,#3575,#3129,.T.);
#4234=EDGE_CURVE('',#3575,#3576,#2230,.T.);
#4235=EDGE_CURVE('',#3576,#3576,#3130,.T.);
#4236=EDGE_CURVE('',#3577,#3578,#2231,.T.);
#4237=EDGE_CURVE('',#3578,#3579,#2232,.T.);
#4238=EDGE_CURVE('',#3580,#3579,#2233,.T.);
#4239=EDGE_CURVE('',#3577,#3580,#2234,.T.);
#4240=EDGE_CURVE('',#3581,#3577,#2235,.T.);
#4241=EDGE_CURVE('',#3582,#3580,#2236,.T.);
#4242=EDGE_CURVE('',#3581,#3582,#2237,.T.);
#4243=EDGE_CURVE('',#3583,#3581,#2238,.T.);
#4244=EDGE_CURVE('',#3584,#3582,#2239,.T.);
#4245=EDGE_CURVE('',#3583,#3584,#2240,.T.);
#4246=EDGE_CURVE('',#3578,#3583,#2241,.T.);
#4247=EDGE_CURVE('',#3579,#3584,#2242,.T.);
#4248=EDGE_CURVE('',#3585,#3585,#3131,.T.);
#4249=EDGE_CURVE('',#3585,#3586,#2243,.T.);
#4250=EDGE_CURVE('',#3586,#3586,#3132,.T.);
#4251=EDGE_CURVE('',#3587,#3587,#3133,.T.);
#4252=EDGE_CURVE('',#3587,#3588,#2244,.T.);
#4253=EDGE_CURVE('',#3588,#3588,#3134,.T.);
#4254=EDGE_CURVE('',#3589,#3589,#3135,.T.);
#4255=EDGE_CURVE('',#3589,#3590,#2245,.T.);
#4256=EDGE_CURVE('',#3590,#3590,#3136,.T.);
#4257=EDGE_CURVE('',#3591,#3591,#3137,.T.);
#4258=EDGE_CURVE('',#3591,#3592,#2246,.T.);
#4259=EDGE_CURVE('',#3592,#3592,#3138,.T.);
#4260=EDGE_CURVE('',#3593,#3594,#2247,.T.);
#4261=EDGE_CURVE('',#3594,#3593,#3139,.T.);
#4262=EDGE_CURVE('',#3595,#3595,#3140,.T.);
#4263=EDGE_CURVE('',#3595,#3596,#2248,.T.);
#4264=EDGE_CURVE('',#3594,#3596,#455,.T.);
#4265=EDGE_CURVE('',#3596,#3593,#456,.T.);
#4266=EDGE_CURVE('',#3597,#3597,#3141,.T.);
#4267=EDGE_CURVE('',#3598,#3599,#2249,.T.);
#4268=EDGE_CURVE('',#3600,#3598,#3142,.T.);
#4269=EDGE_CURVE('',#3599,#3600,#3143,.T.);
#4270=EDGE_CURVE('',#3601,#3601,#3144,.T.);
#4271=EDGE_CURVE('',#3601,#3600,#2250,.T.);
#4272=EDGE_CURVE('',#3599,#3598,#457,.T.);
#4273=EDGE_CURVE('',#3602,#3602,#3145,.T.);
#4274=EDGE_CURVE('',#3603,#3603,#3146,.T.);
#4275=EDGE_CURVE('',#3603,#3597,#2251,.T.);
#4276=EDGE_CURVE('',#3604,#3604,#3147,.T.);
#4277=EDGE_CURVE('',#3604,#3602,#2252,.T.);
#4278=EDGE_CURVE('',#3605,#3606,#2253,.T.);
#4279=EDGE_CURVE('',#3607,#3605,#2254,.T.);
#4280=EDGE_CURVE('',#3607,#3608,#2255,.T.);
#4281=EDGE_CURVE('',#3606,#3608,#2256,.T.);
#4282=EDGE_CURVE('',#3609,#3610,#2257,.T.);
#4283=EDGE_CURVE('',#3611,#3609,#2258,.T.);
#4284=EDGE_CURVE('',#3612,#3611,#2259,.T.);
#4285=EDGE_CURVE('',#3610,#3612,#2260,.T.);
#4286=EDGE_CURVE('',#3612,#3613,#2261,.T.);
#4287=EDGE_CURVE('',#3614,#3611,#2262,.T.);
#4288=EDGE_CURVE('',#3613,#3614,#2263,.T.);
#4289=EDGE_CURVE('',#3613,#3615,#2264,.T.);
#4290=EDGE_CURVE('',#3616,#3614,#2265,.T.);
#4291=EDGE_CURVE('',#3615,#3616,#2266,.T.);
#4292=EDGE_CURVE('',#3615,#3607,#2267,.T.);
#4293=EDGE_CURVE('',#3608,#3616,#2268,.T.);
#4294=EDGE_CURVE('',#3609,#3606,#3148,.T.);
#4295=EDGE_CURVE('',#3617,#3617,#3149,.T.);
#4296=EDGE_CURVE('',#3617,#3618,#2269,.T.);
#4297=EDGE_CURVE('',#3618,#3618,#3150,.T.);
#4298=EDGE_CURVE('',#3610,#3605,#3151,.T.);
#4299=EDGE_CURVE('',#3619,#3619,#3152,.T.);
#4300=EDGE_CURVE('',#3619,#3620,#2270,.T.);
#4301=EDGE_CURVE('',#3620,#3620,#3153,.T.);
#4302=EDGE_CURVE('',#3621,#3621,#3154,.T.);
#4303=EDGE_CURVE('',#3621,#3622,#2271,.T.);
#4304=EDGE_CURVE('',#3622,#3622,#3155,.T.);
#4305=EDGE_CURVE('',#3623,#3623,#3156,.T.);
#4306=EDGE_CURVE('',#3623,#3624,#2272,.T.);
#4307=EDGE_CURVE('',#3624,#3624,#3157,.T.);
#4308=EDGE_CURVE('',#3625,#3625,#3158,.T.);
#4309=EDGE_CURVE('',#3625,#3626,#2273,.T.);
#4310=EDGE_CURVE('',#3626,#3626,#3159,.T.);
#4311=EDGE_CURVE('',#3627,#3627,#3160,.T.);
#4312=EDGE_CURVE('',#3627,#3628,#2274,.T.);
#4313=EDGE_CURVE('',#3628,#3628,#3161,.T.);
#4314=EDGE_CURVE('',#3629,#3629,#3162,.T.);
#4315=EDGE_CURVE('',#3629,#3630,#2275,.T.);
#4316=EDGE_CURVE('',#3630,#3630,#3163,.T.);
#4317=EDGE_CURVE('',#3631,#3631,#3164,.T.);
#4318=EDGE_CURVE('',#3631,#3632,#2276,.T.);
#4319=EDGE_CURVE('',#3632,#3632,#3165,.T.);
#4320=EDGE_CURVE('',#3633,#3633,#3166,.T.);
#4321=EDGE_CURVE('',#3633,#3634,#2277,.T.);
#4322=EDGE_CURVE('',#3634,#3634,#3167,.T.);
#4323=EDGE_CURVE('',#3635,#3635,#3168,.T.);
#4324=EDGE_CURVE('',#3635,#3636,#2278,.T.);
#4325=EDGE_CURVE('',#3636,#3636,#3169,.T.);
#4326=EDGE_CURVE('',#3637,#3637,#3170,.T.);
#4327=EDGE_CURVE('',#3637,#3638,#2279,.T.);
#4328=EDGE_CURVE('',#3638,#3638,#3171,.T.);
#4329=EDGE_CURVE('',#3639,#3639,#3172,.T.);
#4330=EDGE_CURVE('',#3639,#3640,#2280,.T.);
#4331=EDGE_CURVE('',#3640,#3640,#3173,.T.);
#4332=EDGE_CURVE('',#3641,#3641,#3174,.T.);
#4333=EDGE_CURVE('',#3641,#3642,#2281,.T.);
#4334=EDGE_CURVE('',#3642,#3642,#3175,.T.);
#4335=EDGE_CURVE('',#3643,#3643,#3176,.T.);
#4336=EDGE_CURVE('',#3644,#3644,#3177,.T.);
#4337=EDGE_CURVE('',#3644,#3643,#2282,.T.);
#4338=EDGE_CURVE('',#3645,#3645,#3178,.T.);
#4339=EDGE_CURVE('',#3645,#3646,#2283,.T.);
#4340=EDGE_CURVE('',#3646,#3646,#3179,.T.);
#4341=EDGE_CURVE('',#3647,#3647,#3180,.T.);
#4342=EDGE_CURVE('',#3647,#3648,#2284,.T.);
#4343=EDGE_CURVE('',#3648,#3648,#3181,.T.);
#4344=EDGE_CURVE('',#3649,#3649,#3182,.T.);
#4345=EDGE_CURVE('',#3649,#3650,#2285,.T.);
#4346=EDGE_CURVE('',#3650,#3650,#3183,.T.);
#4347=EDGE_CURVE('',#3651,#3651,#3184,.T.);
#4348=EDGE_CURVE('',#3651,#3652,#2286,.T.);
#4349=EDGE_CURVE('',#3652,#3652,#3185,.T.);
#4350=EDGE_CURVE('',#3653,#3653,#3186,.T.);
#4351=EDGE_CURVE('',#3653,#3654,#2287,.T.);
#4352=EDGE_CURVE('',#3654,#3654,#3187,.T.);
#4353=EDGE_CURVE('',#3655,#3656,#2288,.T.);
#4354=EDGE_CURVE('',#3656,#3655,#3188,.T.);
#4355=EDGE_CURVE('',#3657,#3657,#3189,.T.);
#4356=EDGE_CURVE('',#3657,#3658,#2289,.T.);
#4357=EDGE_CURVE('',#3656,#3658,#458,.T.);
#4358=EDGE_CURVE('',#3658,#3655,#459,.T.);
#4359=EDGE_CURVE('',#3659,#3659,#3190,.T.);
#4360=EDGE_CURVE('',#3660,#3661,#2290,.T.);
#4361=EDGE_CURVE('',#3662,#3660,#3191,.T.);
#4362=EDGE_CURVE('',#3661,#3662,#3192,.T.);
#4363=EDGE_CURVE('',#3663,#3663,#3193,.T.);
#4364=EDGE_CURVE('',#3663,#3662,#2291,.T.);
#4365=EDGE_CURVE('',#3661,#3660,#460,.T.);
#4366=EDGE_CURVE('',#3664,#3664,#3194,.T.);
#4367=EDGE_CURVE('',#3665,#3665,#3195,.T.);
#4368=EDGE_CURVE('',#3665,#3659,#2292,.T.);
#4369=EDGE_CURVE('',#3666,#3666,#3196,.T.);
#4370=EDGE_CURVE('',#3666,#3664,#2293,.T.);
#4371=EDGE_CURVE('',#3667,#3668,#2294,.T.);
#4372=EDGE_CURVE('',#3669,#3667,#2295,.T.);
#4373=EDGE_CURVE('',#3669,#3670,#2296,.T.);
#4374=EDGE_CURVE('',#3668,#3670,#2297,.T.);
#4375=EDGE_CURVE('',#3671,#3672,#2298,.T.);
#4376=EDGE_CURVE('',#3673,#3671,#2299,.T.);
#4377=EDGE_CURVE('',#3674,#3673,#2300,.T.);
#4378=EDGE_CURVE('',#3672,#3674,#2301,.T.);
#4379=EDGE_CURVE('',#3674,#3675,#2302,.T.);
#4380=EDGE_CURVE('',#3676,#3673,#2303,.T.);
#4381=EDGE_CURVE('',#3675,#3676,#2304,.T.);
#4382=EDGE_CURVE('',#3675,#3677,#2305,.T.);
#4383=EDGE_CURVE('',#3678,#3676,#2306,.T.);
#4384=EDGE_CURVE('',#3677,#3678,#2307,.T.);
#4385=EDGE_CURVE('',#3677,#3669,#2308,.T.);
#4386=EDGE_CURVE('',#3670,#3678,#2309,.T.);
#4387=EDGE_CURVE('',#3671,#3668,#3197,.T.);
#4388=EDGE_CURVE('',#3679,#3679,#3198,.T.);
#4389=EDGE_CURVE('',#3679,#3680,#2310,.T.);
#4390=EDGE_CURVE('',#3680,#3680,#3199,.T.);
#4391=EDGE_CURVE('',#3672,#3667,#3200,.T.);
#4392=EDGE_CURVE('',#3681,#3681,#3201,.T.);
#4393=EDGE_CURVE('',#3681,#3682,#2311,.T.);
#4394=EDGE_CURVE('',#3682,#3682,#3202,.T.);
#4395=EDGE_CURVE('',#3683,#3683,#3203,.T.);
#4396=EDGE_CURVE('',#3683,#3684,#2312,.T.);
#4397=EDGE_CURVE('',#3684,#3684,#3204,.T.);
#4398=EDGE_CURVE('',#3685,#3685,#3205,.T.);
#4399=EDGE_CURVE('',#3685,#3686,#2313,.T.);
#4400=EDGE_CURVE('',#3686,#3686,#3206,.T.);
#4401=EDGE_CURVE('',#3687,#3687,#3207,.T.);
#4402=EDGE_CURVE('',#3687,#3688,#2314,.T.);
#4403=EDGE_CURVE('',#3688,#3688,#3208,.T.);
#4404=EDGE_CURVE('',#3689,#3689,#3209,.T.);
#4405=EDGE_CURVE('',#3689,#3690,#2315,.T.);
#4406=EDGE_CURVE('',#3690,#3690,#3210,.T.);
#4407=EDGE_CURVE('',#3691,#3691,#3211,.T.);
#4408=EDGE_CURVE('',#3691,#3692,#2316,.T.);
#4409=EDGE_CURVE('',#3692,#3692,#3212,.T.);
#4410=EDGE_CURVE('',#3693,#3693,#3213,.T.);
#4411=EDGE_CURVE('',#3693,#3694,#2317,.T.);
#4412=EDGE_CURVE('',#3694,#3694,#3214,.T.);
#4413=EDGE_CURVE('',#3695,#3695,#3215,.T.);
#4414=EDGE_CURVE('',#3695,#3696,#2318,.T.);
#4415=EDGE_CURVE('',#3696,#3696,#3216,.T.);
#4416=EDGE_CURVE('',#3697,#3697,#3217,.T.);
#4417=EDGE_CURVE('',#3697,#3698,#2319,.T.);
#4418=EDGE_CURVE('',#3698,#3698,#3218,.T.);
#4419=EDGE_CURVE('',#3699,#3699,#3219,.T.);
#4420=EDGE_CURVE('',#3699,#3700,#2320,.T.);
#4421=EDGE_CURVE('',#3700,#3700,#3220,.T.);
#4422=EDGE_CURVE('',#3701,#3701,#3221,.T.);
#4423=EDGE_CURVE('',#3701,#3702,#2321,.T.);
#4424=EDGE_CURVE('',#3702,#3702,#3222,.T.);
#4425=EDGE_CURVE('',#3703,#3703,#3223,.T.);
#4426=EDGE_CURVE('',#3703,#3704,#2322,.T.);
#4427=EDGE_CURVE('',#3704,#3704,#3224,.T.);
#4428=EDGE_CURVE('',#3705,#3705,#3225,.T.);
#4429=EDGE_CURVE('',#3706,#3706,#3226,.T.);
#4430=EDGE_CURVE('',#3706,#3705,#2323,.T.);
#4431=EDGE_CURVE('',#3707,#3707,#3227,.T.);
#4432=EDGE_CURVE('',#3707,#3708,#2324,.T.);
#4433=EDGE_CURVE('',#3708,#3708,#3228,.T.);
#4434=EDGE_CURVE('',#3709,#3709,#3229,.T.);
#4435=EDGE_CURVE('',#3709,#3710,#2325,.T.);
#4436=EDGE_CURVE('',#3710,#3710,#3230,.T.);
#4437=EDGE_CURVE('',#3711,#3711,#3231,.T.);
#4438=EDGE_CURVE('',#3711,#3712,#2326,.T.);
#4439=EDGE_CURVE('',#3712,#3712,#3232,.T.);
#4440=EDGE_CURVE('',#3713,#3713,#3233,.T.);
#4441=EDGE_CURVE('',#3713,#3714,#2327,.T.);
#4442=EDGE_CURVE('',#3714,#3714,#3234,.T.);
#4443=EDGE_CURVE('',#3715,#3715,#3235,.T.);
#4444=EDGE_CURVE('',#3715,#3716,#2328,.T.);
#4445=EDGE_CURVE('',#3716,#3716,#3236,.T.);
#4446=EDGE_CURVE('',#3717,#3718,#2329,.T.);
#4447=EDGE_CURVE('',#3719,#3717,#2330,.T.);
#4448=EDGE_CURVE('',#3720,#3719,#2331,.T.);
#4449=EDGE_CURVE('',#3718,#3720,#2332,.T.);
#4450=EDGE_CURVE('',#3721,#3717,#3237,.T.);
#4451=EDGE_CURVE('',#3721,#3722,#2333,.T.);
#4452=EDGE_CURVE('',#3722,#3719,#2334,.T.);
#4453=EDGE_CURVE('',#3718,#3723,#3238,.T.);
#4454=EDGE_CURVE('',#3720,#3724,#2335,.T.);
#4455=EDGE_CURVE('',#3724,#3723,#2336,.T.);
#4456=EDGE_CURVE('',#3723,#3721,#2337,.T.);
#4457=EDGE_CURVE('',#3724,#3722,#2338,.T.);
#4458=EDGE_CURVE('',#3725,#3725,#3239,.T.);
#4459=EDGE_CURVE('',#3725,#3726,#2339,.T.);
#4460=EDGE_CURVE('',#3726,#3726,#3240,.T.);
#4461=EDGE_CURVE('',#3727,#3727,#3241,.T.);
#4462=EDGE_CURVE('',#3727,#3728,#2340,.T.);
#4463=EDGE_CURVE('',#3728,#3728,#3242,.T.);
#4464=EDGE_CURVE('',#3729,#3729,#3243,.T.);
#4465=EDGE_CURVE('',#3729,#3730,#2341,.T.);
#4466=EDGE_CURVE('',#3730,#3730,#3244,.T.);
#4467=EDGE_CURVE('',#3731,#3731,#3245,.T.);
#4468=EDGE_CURVE('',#3731,#3732,#2342,.T.);
#4469=EDGE_CURVE('',#3732,#3732,#3246,.T.);
#4470=EDGE_CURVE('',#3733,#3733,#3247,.T.);
#4471=EDGE_CURVE('',#3733,#3734,#2343,.T.);
#4472=EDGE_CURVE('',#3734,#3734,#3248,.T.);
#4473=EDGE_CURVE('',#3735,#3735,#3249,.T.);
#4474=EDGE_CURVE('',#3735,#3736,#2344,.T.);
#4475=EDGE_CURVE('',#3736,#3736,#3250,.T.);
#4476=EDGE_CURVE('',#3737,#3737,#3251,.T.);
#4477=EDGE_CURVE('',#3737,#3738,#2345,.T.);
#4478=EDGE_CURVE('',#3738,#3738,#3252,.T.);
#4479=EDGE_CURVE('',#3739,#3739,#3253,.T.);
#4480=EDGE_CURVE('',#3739,#3740,#2346,.T.);
#4481=EDGE_CURVE('',#3740,#3740,#3254,.T.);
#4482=EDGE_CURVE('',#3741,#3741,#3255,.T.);
#4483=EDGE_CURVE('',#3741,#3742,#2347,.T.);
#4484=EDGE_CURVE('',#3742,#3742,#3256,.T.);
#4485=EDGE_CURVE('',#3743,#3743,#3257,.T.);
#4486=EDGE_CURVE('',#3743,#3744,#2348,.T.);
#4487=EDGE_CURVE('',#3744,#3744,#3258,.T.);
#4488=EDGE_CURVE('',#3745,#3745,#3259,.T.);
#4489=EDGE_CURVE('',#3745,#3746,#2349,.T.);
#4490=EDGE_CURVE('',#3746,#3746,#3260,.T.);
#4491=EDGE_CURVE('',#3747,#3747,#3261,.T.);
#4492=EDGE_CURVE('',#3747,#3748,#2350,.T.);
#4493=EDGE_CURVE('',#3748,#3748,#3262,.T.);
#4494=EDGE_CURVE('',#3749,#3749,#3263,.T.);
#4495=EDGE_CURVE('',#3749,#3750,#2351,.T.);
#4496=EDGE_CURVE('',#3750,#3750,#3264,.T.);
#4497=EDGE_CURVE('',#3751,#3751,#3265,.T.);
#4498=EDGE_CURVE('',#3751,#3752,#2352,.T.);
#4499=EDGE_CURVE('',#3752,#3752,#3266,.T.);
#4500=EDGE_CURVE('',#3753,#3753,#3267,.T.);
#4501=EDGE_CURVE('',#3754,#3754,#3268,.T.);
#4502=EDGE_CURVE('',#3754,#3753,#2353,.T.);
#4503=EDGE_CURVE('',#3755,#3755,#3269,.T.);
#4504=EDGE_CURVE('',#3755,#3756,#2354,.T.);
#4505=EDGE_CURVE('',#3756,#3756,#3270,.T.);
#4506=EDGE_CURVE('',#3757,#3757,#3271,.T.);
#4507=EDGE_CURVE('',#3757,#3758,#2355,.T.);
#4508=EDGE_CURVE('',#3758,#3758,#3272,.T.);
#4509=EDGE_CURVE('',#3759,#3759,#3273,.T.);
#4510=EDGE_CURVE('',#3759,#3760,#2356,.T.);
#4511=EDGE_CURVE('',#3760,#3760,#3274,.T.);
#4512=EDGE_CURVE('',#3761,#3761,#3275,.T.);
#4513=EDGE_CURVE('',#3761,#3762,#2357,.T.);
#4514=EDGE_CURVE('',#3762,#3762,#3276,.T.);
#4515=EDGE_CURVE('',#3763,#3763,#3277,.T.);
#4516=EDGE_CURVE('',#3764,#3764,#3278,.T.);
#4517=EDGE_CURVE('',#3764,#3765,#2358,.T.);
#4518=EDGE_CURVE('',#3765,#3765,#3279,.T.);
#4519=EDGE_CURVE('',#3766,#3766,#3280,.T.);
#4520=EDGE_CURVE('',#3767,#3767,#3281,.T.);
#4521=EDGE_CURVE('',#3767,#3768,#2359,.T.);
#4522=EDGE_CURVE('',#3768,#3768,#3282,.T.);
#4523=EDGE_CURVE('',#3769,#3769,#3283,.T.);
#4524=EDGE_CURVE('',#3770,#3770,#3284,.T.);
#4525=EDGE_CURVE('',#3770,#3771,#2360,.T.);
#4526=EDGE_CURVE('',#3771,#3771,#3285,.T.);
#4527=EDGE_CURVE('',#3772,#3772,#3286,.T.);
#4528=EDGE_CURVE('',#3773,#3773,#3287,.T.);
#4529=EDGE_CURVE('',#3773,#3763,#2361,.T.);
#4530=EDGE_CURVE('',#3774,#3774,#3288,.T.);
#4531=EDGE_CURVE('',#3774,#3766,#2362,.T.);
#4532=EDGE_CURVE('',#3775,#3775,#3289,.T.);
#4533=EDGE_CURVE('',#3775,#3769,#2363,.T.);
#4534=EDGE_CURVE('',#3776,#3776,#3290,.T.);
#4535=EDGE_CURVE('',#3776,#3772,#2364,.T.);
#4536=EDGE_CURVE('',#3777,#3778,#2365,.T.);
#4537=EDGE_CURVE('',#3778,#3779,#2366,.T.);
#4538=EDGE_CURVE('',#3780,#3779,#2367,.T.);
#4539=EDGE_CURVE('',#3777,#3780,#2368,.T.);
#4540=EDGE_CURVE('',#3781,#3777,#2369,.T.);
#4541=EDGE_CURVE('',#3782,#3780,#2370,.T.);
#4542=EDGE_CURVE('',#3781,#3782,#2371,.T.);
#4543=EDGE_CURVE('',#3783,#3781,#2372,.T.);
#4544=EDGE_CURVE('',#3784,#3782,#2373,.T.);
#4545=EDGE_CURVE('',#3783,#3784,#2374,.T.);
#4546=EDGE_CURVE('',#3778,#3783,#2375,.T.);
#4547=EDGE_CURVE('',#3779,#3784,#2376,.T.);
#4548=EDGE_CURVE('',#3785,#3785,#3291,.T.);
#4549=EDGE_CURVE('',#3785,#3786,#2377,.T.);
#4550=EDGE_CURVE('',#3786,#3786,#3292,.T.);
#4551=EDGE_CURVE('',#3787,#3787,#3293,.T.);
#4552=EDGE_CURVE('',#3787,#3788,#2378,.T.);
#4553=EDGE_CURVE('',#3788,#3788,#3294,.T.);
#4554=EDGE_CURVE('',#3789,#3790,#2379,.T.);
#4555=EDGE_CURVE('',#3789,#3791,#2380,.T.);
#4556=EDGE_CURVE('',#3792,#3791,#2381,.T.);
#4557=EDGE_CURVE('',#3790,#3792,#2382,.T.);
#4558=EDGE_CURVE('',#3791,#3793,#2383,.T.);
#4559=EDGE_CURVE('',#3793,#3794,#2384,.T.);
#4560=EDGE_CURVE('',#3794,#3792,#2385,.T.);
#4561=EDGE_CURVE('',#3790,#3795,#2386,.T.);
#4562=EDGE_CURVE('',#3796,#3795,#2387,.T.);
#4563=EDGE_CURVE('',#3789,#3796,#2388,.T.);
#4564=EDGE_CURVE('',#3797,#3798,#2389,.T.);
#4565=EDGE_CURVE('',#3797,#3799,#2390,.T.);
#4566=EDGE_CURVE('',#3800,#3799,#2391,.T.);
#4567=EDGE_CURVE('',#3798,#3800,#2392,.T.);
#4568=EDGE_CURVE('',#3798,#3801,#2393,.T.);
#4569=EDGE_CURVE('',#3801,#3802,#2394,.T.);
#4570=EDGE_CURVE('',#3802,#3797,#2395,.T.);
#4571=EDGE_CURVE('',#3802,#3793,#2396,.T.);
#4572=EDGE_CURVE('',#3803,#3796,#2397,.T.);
#4573=EDGE_CURVE('',#3799,#3803,#2398,.T.);
#4574=EDGE_CURVE('',#3804,#3803,#2399,.T.);
#4575=EDGE_CURVE('',#3800,#3804,#2400,.T.);
#4576=EDGE_CURVE('',#3794,#3801,#2401,.T.);
#4577=EDGE_CURVE('',#3795,#3804,#2402,.T.);
#4578=EDGE_CURVE('',#3805,#3805,#3295,.T.);
#4579=EDGE_CURVE('',#3805,#3806,#2403,.T.);
#4580=EDGE_CURVE('',#3806,#3806,#3296,.T.);
#4581=EDGE_CURVE('',#3807,#3807,#3297,.T.);
#4582=EDGE_CURVE('',#3808,#3808,#3298,.T.);
#4583=EDGE_CURVE('',#3808,#3807,#2404,.T.);
#4584=EDGE_CURVE('',#3809,#3809,#3299,.T.);
#4585=EDGE_CURVE('',#3810,#3811,#2405,.T.);
#4586=EDGE_CURVE('',#3812,#3810,#2406,.T.);
#4587=EDGE_CURVE('',#3813,#3812,#2407,.T.);
#4588=EDGE_CURVE('',#3811,#3813,#2408,.T.);
#4589=EDGE_CURVE('',#3809,#3814,#2409,.T.);
#4590=EDGE_CURVE('',#3814,#3814,#3300,.T.);
#4591=EDGE_CURVE('',#3812,#3815,#2410,.T.);
#4592=EDGE_CURVE('',#3816,#3815,#2411,.T.);
#4593=EDGE_CURVE('',#3817,#3816,#2412,.T.);
#4594=EDGE_CURVE('',#3817,#3818,#2413,.T.);
#4595=EDGE_CURVE('',#3819,#3818,#2414,.T.);
#4596=EDGE_CURVE('',#3819,#3820,#2415,.T.);
#4597=EDGE_CURVE('',#3813,#3820,#2416,.T.);
#4598=EDGE_CURVE('',#3810,#3821,#2417,.T.);
#4599=EDGE_CURVE('',#3821,#3822,#2418,.T.);
#4600=EDGE_CURVE('',#3822,#3823,#2419,.T.);
#4601=EDGE_CURVE('',#3823,#3824,#2420,.T.);
#4602=EDGE_CURVE('',#3824,#3825,#2421,.T.);
#4603=EDGE_CURVE('',#3815,#3825,#2422,.T.);
#4604=EDGE_CURVE('',#3826,#3826,#3301,.T.);
#4605=EDGE_CURVE('',#3826,#3827,#2423,.T.);
#4606=EDGE_CURVE('',#3827,#3827,#3302,.T.);
#4607=EDGE_CURVE('',#3828,#3828,#3303,.T.);
#4608=EDGE_CURVE('',#3829,#3829,#3304,.T.);
#4609=EDGE_CURVE('',#3829,#3828,#2424,.T.);
#4610=EDGE_CURVE('',#3830,#3830,#3305,.T.);
#4611=EDGE_CURVE('',#3831,#3817,#2425,.T.);
#4612=EDGE_CURVE('',#3832,#3831,#2426,.T.);
#4613=EDGE_CURVE('',#3818,#3832,#2427,.T.);
#4614=EDGE_CURVE('',#3830,#3833,#2428,.T.);
#4615=EDGE_CURVE('',#3833,#3833,#3306,.T.);
#4616=EDGE_CURVE('',#3832,#3834,#2429,.T.);
#4617=EDGE_CURVE('',#3819,#3834,#2430,.T.);
#4618=EDGE_CURVE('',#3835,#3831,#2431,.T.);
#4619=EDGE_CURVE('',#3834,#3835,#2432,.T.);
#4620=EDGE_CURVE('',#3836,#3836,#3307,.T.);
#4621=EDGE_CURVE('',#3836,#3837,#2433,.T.);
#4622=EDGE_CURVE('',#3837,#3837,#3308,.T.);
#4623=EDGE_CURVE('',#3838,#3838,#3309,.T.);
#4624=EDGE_CURVE('',#3839,#3839,#3310,.T.);
#4625=EDGE_CURVE('',#3839,#3838,#2434,.T.);
#4626=EDGE_CURVE('',#3840,#3840,#3311,.T.);
#4627=EDGE_CURVE('',#3841,#3823,#2435,.T.);
#4628=EDGE_CURVE('',#3842,#3841,#2436,.T.);
#4629=EDGE_CURVE('',#3824,#3842,#2437,.T.);
#4630=EDGE_CURVE('',#3840,#3843,#2438,.T.);
#4631=EDGE_CURVE('',#3843,#3843,#3312,.T.);
#4632=EDGE_CURVE('',#3841,#3844,#2439,.T.);
#4633=EDGE_CURVE('',#3845,#3844,#2440,.T.);
#4634=EDGE_CURVE('',#3845,#3842,#2441,.T.);
#4635=EDGE_CURVE('',#3844,#3822,#2442,.T.);
#4636=EDGE_CURVE('',#3846,#3846,#3313,.T.);
#4637=EDGE_CURVE('',#3846,#3847,#2443,.T.);
#4638=EDGE_CURVE('',#3847,#3847,#3314,.T.);
#4639=EDGE_CURVE('',#3848,#3848,#3315,.T.);
#4640=EDGE_CURVE('',#3849,#3849,#3316,.T.);
#4641=EDGE_CURVE('',#3849,#3848,#2444,.T.);
#4642=EDGE_CURVE('',#3850,#3850,#3317,.T.);
#4643=EDGE_CURVE('',#3851,#3852,#2445,.T.);
#4644=EDGE_CURVE('',#3853,#3851,#2446,.T.);
#4645=EDGE_CURVE('',#3854,#3853,#2447,.T.);
#4646=EDGE_CURVE('',#3852,#3854,#2448,.T.);
#4647=EDGE_CURVE('',#3850,#3855,#2449,.T.);
#4648=EDGE_CURVE('',#3855,#3855,#3318,.T.);
#4649=EDGE_CURVE('',#3856,#3816,#2450,.T.);
#4650=EDGE_CURVE('',#3854,#3856,#2451,.T.);
#4651=EDGE_CURVE('',#3853,#3857,#2452,.T.);
#4652=EDGE_CURVE('',#3857,#3835,#2453,.T.);
#4653=EDGE_CURVE('',#3858,#3851,#2454,.T.);
#4654=EDGE_CURVE('',#3857,#3858,#2455,.T.);
#4655=EDGE_CURVE('',#3859,#3860,#2456,.T.);
#4656=EDGE_CURVE('',#3859,#3861,#2457,.T.);
#4657=EDGE_CURVE('',#3862,#3861,#2458,.T.);
#4658=EDGE_CURVE('',#3860,#3862,#2459,.T.);
#4659=EDGE_CURVE('',#3860,#3863,#2460,.T.);
#4660=EDGE_CURVE('',#3864,#3862,#2461,.T.);
#4661=EDGE_CURVE('',#3863,#3864,#2462,.T.);
#4662=EDGE_CURVE('',#3863,#3865,#2463,.T.);
#4663=EDGE_CURVE('',#3866,#3864,#2464,.T.);
#4664=EDGE_CURVE('',#3865,#3866,#2465,.T.);
#4665=EDGE_CURVE('',#3865,#3859,#2466,.T.);
#4666=EDGE_CURVE('',#3861,#3866,#2467,.T.);
#4667=EDGE_CURVE('',#3867,#3811,#2468,.T.);
#4668=EDGE_CURVE('',#3821,#3867,#2469,.T.);
#4669=EDGE_CURVE('',#3867,#3820,#2470,.T.);
#4670=EDGE_CURVE('',#3858,#3868,#2471,.T.);
#4671=EDGE_CURVE('',#3845,#3868,#2472,.T.);
#4672=EDGE_CURVE('',#3852,#3868,#2473,.T.);
#4673=EDGE_CURVE('',#3825,#3856,#2474,.T.);
#4674=EDGE_CURVE('',#3869,#3870,#2475,.T.);
#4675=EDGE_CURVE('',#3870,#3871,#2476,.T.);
#4676=EDGE_CURVE('',#3872,#3871,#2477,.T.);
#4677=EDGE_CURVE('',#3869,#3872,#2478,.T.);
#4678=EDGE_CURVE('',#3873,#3869,#2479,.T.);
#4679=EDGE_CURVE('',#3874,#3872,#2480,.T.);
#4680=EDGE_CURVE('',#3873,#3874,#2481,.T.);
#4681=EDGE_CURVE('',#3875,#3873,#2482,.T.);
#4682=EDGE_CURVE('',#3876,#3874,#2483,.T.);
#4683=EDGE_CURVE('',#3875,#3876,#2484,.T.);
#4684=EDGE_CURVE('',#3870,#3875,#2485,.T.);
#4685=EDGE_CURVE('',#3871,#3876,#2486,.T.);
#4686=EDGE_CURVE('',#3877,#3878,#2487,.T.);
#4687=EDGE_CURVE('',#3878,#3879,#2488,.T.);
#4688=EDGE_CURVE('',#3880,#3879,#2489,.T.);
#4689=EDGE_CURVE('',#3877,#3880,#2490,.T.);
#4690=EDGE_CURVE('',#3881,#3877,#2491,.T.);
#4691=EDGE_CURVE('',#3882,#3880,#2492,.T.);
#4692=EDGE_CURVE('',#3881,#3882,#2493,.T.);
#4693=EDGE_CURVE('',#3883,#3881,#2494,.T.);
#4694=EDGE_CURVE('',#3884,#3882,#2495,.T.);
#4695=EDGE_CURVE('',#3883,#3884,#2496,.T.);
#4696=EDGE_CURVE('',#3878,#3883,#2497,.T.);
#4697=EDGE_CURVE('',#3879,#3884,#2498,.T.);
#4698=EDGE_CURVE('',#3885,#3886,#2499,.T.);
#4699=EDGE_CURVE('',#3886,#3887,#2500,.T.);
#4700=EDGE_CURVE('',#3887,#3888,#2501,.T.);
#4701=EDGE_CURVE('',#3885,#3888,#2502,.T.);
#4702=EDGE_CURVE('',#3886,#3889,#2503,.T.);
#4703=EDGE_CURVE('',#3889,#3890,#2504,.T.);
#4704=EDGE_CURVE('',#3890,#3887,#2505,.T.);
#4705=EDGE_CURVE('',#3889,#3891,#2506,.T.);
#4706=EDGE_CURVE('',#3891,#3892,#2507,.T.);
#4707=EDGE_CURVE('',#3892,#3890,#2508,.T.);
#4708=EDGE_CURVE('',#3891,#3893,#2509,.T.);
#4709=EDGE_CURVE('',#3893,#3894,#2510,.T.);
#4710=EDGE_CURVE('',#3894,#3892,#2511,.T.);
#4711=EDGE_CURVE('',#3893,#3895,#2512,.T.);
#4712=EDGE_CURVE('',#3895,#3896,#2513,.T.);
#4713=EDGE_CURVE('',#3896,#3894,#2514,.T.);
#4714=EDGE_CURVE('',#3895,#3885,#2515,.T.);
#4715=EDGE_CURVE('',#3888,#3896,#2516,.T.);
#4716=EDGE_CURVE('',#3897,#3897,#3319,.T.);
#4717=EDGE_CURVE('',#3898,#3898,#3320,.T.);
#4718=EDGE_CURVE('',#3899,#3899,#3321,.T.);
#4719=EDGE_CURVE('',#3899,#3898,#2517,.T.);
#4720=EDGE_CURVE('',#3900,#3900,#3322,.T.);
#4721=EDGE_CURVE('',#3900,#3899,#2518,.T.);
#4722=EDGE_CURVE('',#3901,#3901,#3323,.T.);
#4723=EDGE_CURVE('',#3901,#3900,#2519,.T.);
#4724=EDGE_CURVE('',#3902,#3902,#3324,.T.);
#4725=EDGE_CURVE('',#3903,#3903,#3325,.F.);
#4726=EDGE_CURVE('',#3903,#3902,#2520,.T.);
#4727=EDGE_CURVE('',#3897,#3903,#2521,.T.);
#4728=EDGE_CURVE('',#3904,#3905,#3326,.T.);
#4729=EDGE_CURVE('',#3905,#3904,#3327,.T.);
#4730=EDGE_CURVE('',#3905,#3906,#3328,.T.);
#4731=EDGE_CURVE('',#3907,#3906,#3329,.T.);
#4732=EDGE_CURVE('',#3906,#3907,#3330,.T.);
#4733=EDGE_CURVE('',#3907,#3908,#2522,.T.);
#4734=EDGE_CURVE('',#3908,#3908,#3331,.T.);
#4735=EDGE_CURVE('',#3909,#3909,#3332,.T.);
#4736=EDGE_CURVE('',#3909,#3910,#2523,.T.);
#4737=EDGE_CURVE('',#3910,#3910,#3333,.T.);
#4738=EDGE_CURVE('',#3910,#3911,#2524,.T.);
#4739=EDGE_CURVE('',#3911,#3911,#3334,.T.);
#4740=EDGE_CURVE('',#3912,#3912,#3335,.T.);
#4741=EDGE_CURVE('',#3912,#3904,#2525,.T.);
#4742=EDGE_CURVE('',#3913,#3913,#3336,.T.);
#4743=EDGE_CURVE('',#3913,#3909,#2526,.T.);
#4744=EDGE_CURVE('',#3914,#3915,#3337,.T.);
#4745=EDGE_CURVE('',#3915,#3914,#3338,.T.);
#4746=EDGE_CURVE('',#3915,#3916,#3339,.T.);
#4747=EDGE_CURVE('',#3917,#3916,#3340,.T.);
#4748=EDGE_CURVE('',#3916,#3917,#3341,.T.);
#4749=EDGE_CURVE('',#3918,#3918,#3342,.T.);
#4750=EDGE_CURVE('',#3918,#3917,#2527,.T.);
#4751=EDGE_CURVE('',#3919,#3919,#3343,.T.);
#4752=EDGE_CURVE('',#3920,#3920,#3344,.T.);
#4753=EDGE_CURVE('',#3921,#3921,#3345,.T.);
#4754=EDGE_CURVE('',#3921,#3919,#2528,.T.);
#4755=EDGE_CURVE('',#3922,#3922,#3346,.T.);
#4756=EDGE_CURVE('',#3922,#3921,#2529,.T.);
#4757=EDGE_CURVE('',#3923,#3923,#3347,.T.);
#4758=EDGE_CURVE('',#3923,#3922,#2530,.T.);
#4759=EDGE_CURVE('',#3914,#3920,#2531,.T.);
#4760=EDGE_CURVE('',#3924,#3925,#3348,.T.);
#4761=EDGE_CURVE('',#3926,#3927,#3349,.T.);
#4762=EDGE_CURVE('',#3928,#3929,#3350,.T.);
#4763=EDGE_CURVE('',#3930,#3931,#3351,.T.);
#4764=EDGE_CURVE('',#3932,#3933,#3352,.T.);
#4765=EDGE_CURVE('',#3934,#3935,#3353,.T.);
#4766=EDGE_CURVE('',#3936,#3937,#3354,.T.);
#4767=EDGE_CURVE('',#3938,#3939,#343,.T.);
#4768=EDGE_CURVE('',#3940,#3938,#3355,.T.);
#4769=EDGE_CURVE('',#3941,#3940,#344,.T.);
#4770=EDGE_CURVE('',#3939,#3941,#3356,.T.);
#4771=EDGE_CURVE('',#3942,#3940,#3357,.T.);
#4772=EDGE_CURVE('',#3942,#3943,#345,.T.);
#4773=EDGE_CURVE('',#3944,#3943,#3358,.T.);
#4774=EDGE_CURVE('',#3944,#3945,#346,.T.);
#4775=EDGE_CURVE('',#3946,#3945,#3359,.T.);
#4776=EDGE_CURVE('',#3946,#3947,#2532,.T.);
#4777=EDGE_CURVE('',#3947,#3947,#3360,.T.);
#4778=EDGE_CURVE('',#3948,#3946,#3361,.T.);
#4779=EDGE_CURVE('',#3948,#3949,#347,.T.);
#4780=EDGE_CURVE('',#3950,#3949,#3362,.T.);
#4781=EDGE_CURVE('',#3950,#3951,#348,.T.);
#4782=EDGE_CURVE('',#3952,#3951,#3363,.T.);
#4783=EDGE_CURVE('',#3952,#3953,#349,.T.);
#4784=EDGE_CURVE('',#3954,#3953,#3364,.T.);
#4785=EDGE_CURVE('',#3954,#3955,#350,.T.);
#4786=EDGE_CURVE('',#3941,#3955,#3365,.T.);
#4787=EDGE_CURVE('',#3938,#3956,#3366,.T.);
#4788=EDGE_CURVE('',#3956,#3942,#3367,.T.);
#4789=EDGE_CURVE('',#3957,#3956,#351,.T.);
#4790=EDGE_CURVE('',#3943,#3957,#3368,.T.);
#4791=EDGE_CURVE('',#3957,#3958,#3369,.T.);
#4792=EDGE_CURVE('',#3958,#3944,#3370,.T.);
#4793=EDGE_CURVE('',#3959,#3958,#352,.T.);
#4794=EDGE_CURVE('',#3945,#3959,#3371,.T.);
#4795=EDGE_CURVE('',#3959,#3960,#3372,.T.);
#4796=EDGE_CURVE('',#3960,#3961,#3373,.T.);
#4797=EDGE_CURVE('',#3961,#3948,#3374,.T.);
#4798=EDGE_CURVE('',#3962,#3961,#353,.T.);
#4799=EDGE_CURVE('',#3949,#3962,#3375,.T.);
#4800=EDGE_CURVE('',#3962,#3963,#3376,.T.);
#4801=EDGE_CURVE('',#3963,#3950,#3377,.T.);
#4802=EDGE_CURVE('',#3964,#3963,#354,.T.);
#4803=EDGE_CURVE('',#3951,#3964,#3378,.T.);
#4804=EDGE_CURVE('',#3964,#3965,#3379,.T.);
#4805=EDGE_CURVE('',#3965,#3952,#3380,.T.);
#4806=EDGE_CURVE('',#3966,#3965,#355,.T.);
#4807=EDGE_CURVE('',#3953,#3966,#3381,.T.);
#4808=EDGE_CURVE('',#3967,#3967,#3382,.T.);
#4809=EDGE_CURVE('',#3967,#3960,#2533,.T.);
#4810=EDGE_CURVE('',#3968,#3939,#3383,.T.);
#4811=EDGE_CURVE('',#3968,#3969,#356,.T.);
#4812=EDGE_CURVE('',#3966,#3969,#3384,.T.);
#4813=EDGE_CURVE('',#3955,#3968,#3385,.T.);
#4814=EDGE_CURVE('',#3969,#3954,#3386,.T.);
#4815=EDGE_CURVE('',#3970,#3970,#3387,.T.);
#4816=EDGE_CURVE('',#3971,#3971,#3388,.T.);
#4817=EDGE_CURVE('',#3972,#3972,#3389,.T.);
#4818=EDGE_CURVE('',#3972,#3970,#2534,.T.);
#4819=EDGE_CURVE('',#3973,#3973,#3390,.T.);
#4820=EDGE_CURVE('',#3973,#3971,#2535,.T.);
#4821=EDGE_CURVE('',#3974,#3974,#3391,.T.);
#4822=EDGE_CURVE('',#3975,#3975,#3392,.T.);
#4823=EDGE_CURVE('',#3976,#3976,#3393,.T.);
#4824=EDGE_CURVE('',#3976,#3974,#2536,.T.);
#4825=EDGE_CURVE('',#3977,#3977,#3394,.T.);
#4826=EDGE_CURVE('',#3977,#3975,#2537,.T.);
#4827=EDGE_CURVE('',#3978,#3979,#3395,.T.);
#4828=EDGE_CURVE('',#3979,#3978,#3396,.T.);
#4829=EDGE_CURVE('',#3979,#3980,#3397,.T.);
#4830=EDGE_CURVE('',#3981,#3980,#3398,.T.);
#4831=EDGE_CURVE('',#3980,#3981,#3399,.T.);
#4832=EDGE_CURVE('',#3981,#3982,#2538,.T.);
#4833=EDGE_CURVE('',#3982,#3982,#3400,.T.);
#4834=EDGE_CURVE('',#3983,#3983,#3401,.T.);
#4835=EDGE_CURVE('',#3983,#3984,#2539,.T.);
#4836=EDGE_CURVE('',#3984,#3984,#3402,.T.);
#4837=EDGE_CURVE('',#3984,#3985,#2540,.T.);
#4838=EDGE_CURVE('',#3985,#3985,#3403,.T.);
#4839=EDGE_CURVE('',#3986,#3986,#3404,.T.);
#4840=EDGE_CURVE('',#3986,#3978,#2541,.T.);
#4841=EDGE_CURVE('',#3987,#3987,#3405,.T.);
#4842=EDGE_CURVE('',#3987,#3983,#2542,.T.);
#4843=EDGE_CURVE('',#3988,#3989,#3406,.T.);
#4844=EDGE_CURVE('',#3989,#3988,#3407,.T.);
#4845=EDGE_CURVE('',#3989,#3990,#3408,.T.);
#4846=EDGE_CURVE('',#3991,#3990,#3409,.T.);
#4847=EDGE_CURVE('',#3990,#3991,#3410,.T.);
#4848=EDGE_CURVE('',#3992,#3992,#3411,.T.);
#4849=EDGE_CURVE('',#3992,#3991,#2543,.T.);
#4850=EDGE_CURVE('',#3993,#3993,#3412,.T.);
#4851=EDGE_CURVE('',#3994,#3994,#3413,.T.);
#4852=EDGE_CURVE('',#3995,#3995,#3414,.T.);
#4853=EDGE_CURVE('',#3995,#3993,#2544,.T.);
#4854=EDGE_CURVE('',#3996,#3996,#3415,.T.);
#4855=EDGE_CURVE('',#3996,#3995,#2545,.T.);
#4856=EDGE_CURVE('',#3997,#3997,#3416,.T.);
#4857=EDGE_CURVE('',#3997,#3996,#2546,.T.);
#4858=EDGE_CURVE('',#3988,#3994,#2547,.T.);
#4859=EDGE_CURVE('',#3998,#3999,#3417,.T.);
#4860=EDGE_CURVE('',#4000,#4001,#3418,.T.);
#4861=EDGE_CURVE('',#4002,#4003,#3419,.T.);
#4862=EDGE_CURVE('',#4004,#4005,#3420,.T.);
#4863=EDGE_CURVE('',#4006,#4007,#3421,.T.);
#4864=EDGE_CURVE('',#4008,#4009,#3422,.T.);
#4865=EDGE_CURVE('',#4010,#4011,#3423,.T.);
#4866=EDGE_CURVE('',#4012,#4013,#3424,.T.);
#4867=EDGE_CURVE('',#4014,#4015,#357,.T.);
#4868=EDGE_CURVE('',#4016,#4014,#3425,.T.);
#4869=EDGE_CURVE('',#4017,#4016,#358,.T.);
#4870=EDGE_CURVE('',#4015,#4017,#3426,.T.);
#4871=EDGE_CURVE('',#4018,#4016,#3427,.T.);
#4872=EDGE_CURVE('',#4018,#4019,#359,.T.);
#4873=EDGE_CURVE('',#4020,#4019,#3428,.T.);
#4874=EDGE_CURVE('',#4020,#4021,#360,.T.);
#4875=EDGE_CURVE('',#4022,#4021,#3429,.T.);
#4876=EDGE_CURVE('',#4022,#4023,#361,.T.);
#4877=EDGE_CURVE('',#4023,#4024,#2548,.T.);
#4878=EDGE_CURVE('',#4024,#4024,#3430,.T.);
#4879=EDGE_CURVE('',#4023,#4025,#362,.T.);
#4880=EDGE_CURVE('',#4026,#4025,#3431,.T.);
#4881=EDGE_CURVE('',#4026,#4027,#363,.T.);
#4882=EDGE_CURVE('',#4028,#4027,#3432,.T.);
#4883=EDGE_CURVE('',#4028,#4029,#364,.T.);
#4884=EDGE_CURVE('',#4030,#4029,#3433,.T.);
#4885=EDGE_CURVE('',#4030,#4031,#365,.T.);
#4886=EDGE_CURVE('',#4032,#4031,#3434,.T.);
#4887=EDGE_CURVE('',#4032,#4033,#366,.T.);
#4888=EDGE_CURVE('',#4017,#4033,#3435,.T.);
#4889=EDGE_CURVE('',#4014,#4034,#3436,.T.);
#4890=EDGE_CURVE('',#4034,#4018,#3437,.T.);
#4891=EDGE_CURVE('',#4035,#4034,#367,.T.);
#4892=EDGE_CURVE('',#4019,#4035,#3438,.T.);
#4893=EDGE_CURVE('',#4035,#4036,#3439,.T.);
#4894=EDGE_CURVE('',#4036,#4020,#3440,.T.);
#4895=EDGE_CURVE('',#4037,#4036,#368,.T.);
#4896=EDGE_CURVE('',#4021,#4037,#3441,.T.);
#4897=EDGE_CURVE('',#4037,#4038,#3442,.T.);
#4898=EDGE_CURVE('',#4038,#4022,#3443,.T.);
#4899=EDGE_CURVE('',#4039,#4040,#369,.T.);
#4900=EDGE_CURVE('',#4025,#4039,#3444,.T.);
#4901=EDGE_CURVE('',#4040,#4038,#370,.T.);
#4902=EDGE_CURVE('',#4039,#4041,#3445,.T.);
#4903=EDGE_CURVE('',#4041,#4026,#3446,.T.);
#4904=EDGE_CURVE('',#4042,#4041,#371,.T.);
#4905=EDGE_CURVE('',#4027,#4042,#3447,.T.);
#4906=EDGE_CURVE('',#4042,#4043,#3448,.T.);
#4907=EDGE_CURVE('',#4043,#4028,#3449,.T.);
#4908=EDGE_CURVE('',#4044,#4043,#372,.T.);
#4909=EDGE_CURVE('',#4029,#4044,#3450,.T.);
#4910=EDGE_CURVE('',#4044,#4045,#3451,.T.);
#4911=EDGE_CURVE('',#4045,#4030,#3452,.T.);
#4912=EDGE_CURVE('',#4046,#4045,#373,.T.);
#4913=EDGE_CURVE('',#4031,#4046,#3453,.T.);
#4914=EDGE_CURVE('',#4047,#4047,#3454,.T.);
#4915=EDGE_CURVE('',#4047,#4040,#2549,.T.);
#4916=EDGE_CURVE('',#4048,#4015,#3455,.T.);
#4917=EDGE_CURVE('',#4048,#4049,#374,.T.);
#4918=EDGE_CURVE('',#4046,#4049,#3456,.T.);
#4919=EDGE_CURVE('',#4033,#4048,#3457,.T.);
#4920=EDGE_CURVE('',#4049,#4032,#3458,.T.);
#4921=EDGE_CURVE('',#4050,#4050,#3459,.T.);
#4922=EDGE_CURVE('',#4051,#4051,#3460,.T.);
#4923=EDGE_CURVE('',#4052,#4052,#3461,.T.);
#4924=EDGE_CURVE('',#4052,#4050,#2550,.T.);
#4925=EDGE_CURVE('',#4053,#4053,#3462,.T.);
#4926=EDGE_CURVE('',#4053,#4051,#2551,.T.);
#4927=EDGE_CURVE('',#4054,#4054,#3463,.T.);
#4928=EDGE_CURVE('',#4055,#4055,#3464,.T.);
#4929=EDGE_CURVE('',#4056,#4056,#3465,.T.);
#4930=EDGE_CURVE('',#4056,#4054,#2552,.T.);
#4931=EDGE_CURVE('',#4057,#4057,#3466,.T.);
#4932=EDGE_CURVE('',#4057,#4055,#2553,.T.);
#4933=EDGE_CURVE('',#4058,#4058,#3467,.T.);
#4934=EDGE_CURVE('',#4059,#4059,#3468,.T.);
#4935=EDGE_CURVE('',#4059,#4058,#2554,.T.);
#4936=EDGE_CURVE('',#4060,#4060,#3469,.T.);
#4937=EDGE_CURVE('',#4060,#4059,#2555,.T.);
#4938=EDGE_CURVE('',#4061,#4061,#3470,.T.);
#4939=EDGE_CURVE('',#4061,#4060,#2556,.T.);
#4940=EDGE_CURVE('',#4062,#4062,#3471,.T.);
#4941=EDGE_CURVE('',#4063,#4063,#3472,.F.);
#4942=EDGE_CURVE('',#4063,#4062,#2557,.T.);
#4943=EDGE_CURVE('',#4064,#4064,#3473,.F.);
#4944=EDGE_CURVE('',#4064,#4063,#2558,.T.);
#4945=EDGE_CURVE('',#4065,#4065,#3474,.T.);
#4946=EDGE_CURVE('',#4065,#4064,#2559,.T.);
#4947=EDGE_CURVE('',#4066,#4067,#2560,.T.);
#4948=EDGE_CURVE('',#4067,#4068,#2561,.T.);
#4949=EDGE_CURVE('',#4068,#4069,#2562,.T.);
#4950=EDGE_CURVE('',#4066,#4069,#2563,.T.);
#4951=EDGE_CURVE('',#4067,#4070,#2564,.T.);
#4952=EDGE_CURVE('',#4070,#4071,#2565,.T.);
#4953=EDGE_CURVE('',#4071,#4068,#2566,.T.);
#4954=EDGE_CURVE('',#4070,#4072,#2567,.T.);
#4955=EDGE_CURVE('',#4072,#4073,#2568,.T.);
#4956=EDGE_CURVE('',#4073,#4071,#2569,.T.);
#4957=EDGE_CURVE('',#4072,#4074,#2570,.T.);
#4958=EDGE_CURVE('',#4074,#4075,#2571,.T.);
#4959=EDGE_CURVE('',#4075,#4073,#2572,.T.);
#4960=EDGE_CURVE('',#4074,#4076,#2573,.T.);
#4961=EDGE_CURVE('',#4076,#4077,#2574,.T.);
#4962=EDGE_CURVE('',#4077,#4075,#2575,.T.);
#4963=EDGE_CURVE('',#4076,#4066,#2576,.T.);
#4964=EDGE_CURVE('',#4069,#4077,#2577,.T.);
#4965=EDGE_CURVE('',#4078,#4079,#2578,.T.);
#4966=EDGE_CURVE('',#4079,#4080,#2579,.T.);
#4967=EDGE_CURVE('',#4080,#4081,#2580,.T.);
#4968=EDGE_CURVE('',#4078,#4081,#2581,.T.);
#4969=EDGE_CURVE('',#4079,#4082,#2582,.T.);
#4970=EDGE_CURVE('',#4082,#4083,#2583,.T.);
#4971=EDGE_CURVE('',#4083,#4080,#2584,.T.);
#4972=EDGE_CURVE('',#4082,#4084,#2585,.T.);
#4973=EDGE_CURVE('',#4084,#4085,#2586,.T.);
#4974=EDGE_CURVE('',#4085,#4083,#2587,.T.);
#4975=EDGE_CURVE('',#4084,#4086,#2588,.T.);
#4976=EDGE_CURVE('',#4086,#4087,#2589,.T.);
#4977=EDGE_CURVE('',#4087,#4085,#2590,.T.);
#4978=EDGE_CURVE('',#4086,#4088,#2591,.T.);
#4979=EDGE_CURVE('',#4088,#4089,#2592,.T.);
#4980=EDGE_CURVE('',#4089,#4087,#2593,.T.);
#4981=EDGE_CURVE('',#4088,#4078,#2594,.T.);
#4982=EDGE_CURVE('',#4081,#4089,#2595,.T.);
#4983=EDGE_CURVE('',#4090,#4090,#3475,.T.);
#4984=EDGE_CURVE('',#4091,#4091,#3476,.T.);
#4985=EDGE_CURVE('',#4092,#4092,#3477,.T.);
#4986=EDGE_CURVE('',#4092,#4091,#2596,.T.);
#4987=EDGE_CURVE('',#4093,#4093,#3478,.T.);
#4988=EDGE_CURVE('',#4093,#4092,#2597,.T.);
#4989=EDGE_CURVE('',#4094,#4094,#3479,.T.);
#4990=EDGE_CURVE('',#4094,#4093,#2598,.T.);
#4991=EDGE_CURVE('',#4095,#4095,#3480,.T.);
#4992=EDGE_CURVE('',#4096,#4096,#3481,.F.);
#4993=EDGE_CURVE('',#4096,#4095,#2599,.T.);
#4994=EDGE_CURVE('',#4090,#4096,#2600,.T.);
#4995=EDGE_CURVE('',#4097,#4097,#3482,.T.);
#4996=EDGE_CURVE('',#4097,#4098,#2601,.T.);
#4997=EDGE_CURVE('',#4098,#4098,#3483,.T.);
#4998=EDGE_CURVE('',#4099,#4099,#3484,.T.);
#4999=EDGE_CURVE('',#4099,#4100,#2602,.T.);
#5000=EDGE_CURVE('',#4100,#4100,#3485,.T.);
#5001=EDGE_CURVE('',#4101,#4101,#3486,.T.);
#5002=EDGE_CURVE('',#4101,#4102,#2603,.T.);
#5003=EDGE_CURVE('',#4102,#4102,#3487,.T.);
#5004=EDGE_CURVE('',#4103,#4103,#3488,.T.);
#5005=EDGE_CURVE('',#4103,#4104,#2604,.T.);
#5006=EDGE_CURVE('',#4104,#4104,#3489,.T.);
#5007=EDGE_CURVE('',#4105,#4105,#3490,.T.);
#5008=EDGE_CURVE('',#4105,#4106,#2605,.T.);
#5009=EDGE_CURVE('',#4106,#4106,#3491,.T.);
#5010=EDGE_CURVE('',#4107,#4107,#3492,.T.);
#5011=EDGE_CURVE('',#4107,#4108,#2606,.T.);
#5012=EDGE_CURVE('',#4108,#4108,#3493,.T.);
#5013=EDGE_CURVE('',#4109,#4109,#3494,.T.);
#5014=EDGE_CURVE('',#4109,#4110,#2607,.T.);
#5015=EDGE_CURVE('',#4110,#4110,#3495,.T.);
#5016=EDGE_CURVE('',#4111,#4112,#2608,.T.);
#5017=EDGE_CURVE('',#4111,#4112,#3496,.T.);
#5018=EDGE_CURVE('',#4113,#4111,#375,.T.);
#5019=EDGE_CURVE('',#4114,#4113,#3497,.T.);
#5020=EDGE_CURVE('',#4114,#4115,#2609,.T.);
#5021=EDGE_CURVE('',#4116,#4115,#376,.T.);
#5022=EDGE_CURVE('',#4115,#4116,#377,.T.);
#5023=EDGE_CURVE('',#4117,#4114,#3498,.T.);
#5024=EDGE_CURVE('',#4112,#4117,#378,.T.);
#5025=EDGE_CURVE('',#4117,#4113,#2610,.T.);
#5026=EDGE_CURVE('',#4118,#4118,#3499,.T.);
#5027=EDGE_CURVE('',#4118,#4119,#2611,.T.);
#5028=EDGE_CURVE('',#4119,#4119,#3500,.T.);
#5029=EDGE_CURVE('',#4120,#4120,#3501,.T.);
#5030=EDGE_CURVE('',#4120,#4121,#2612,.T.);
#5031=EDGE_CURVE('',#4121,#4121,#3502,.T.);
#5032=EDGE_CURVE('',#4122,#4123,#2613,.T.);
#5033=EDGE_CURVE('',#4122,#4123,#3503,.T.);
#5034=EDGE_CURVE('',#4124,#4122,#379,.T.);
#5035=EDGE_CURVE('',#4125,#4124,#3504,.T.);
#5036=EDGE_CURVE('',#4125,#4126,#2614,.T.);
#5037=EDGE_CURVE('',#4127,#4126,#380,.T.);
#5038=EDGE_CURVE('',#4126,#4127,#381,.T.);
#5039=EDGE_CURVE('',#4128,#4125,#3505,.T.);
#5040=EDGE_CURVE('',#4123,#4128,#382,.T.);
#5041=EDGE_CURVE('',#4128,#4124,#2615,.T.);
#5042=EDGE_CURVE('',#4129,#4129,#3506,.T.);
#5043=EDGE_CURVE('',#4129,#4130,#2616,.T.);
#5044=EDGE_CURVE('',#4130,#4130,#3507,.T.);
#5045=EDGE_CURVE('',#4131,#4131,#3508,.T.);
#5046=EDGE_CURVE('',#4131,#4132,#2617,.T.);
#5047=EDGE_CURVE('',#4132,#4132,#3509,.T.);
#5048=EDGE_CURVE('',#4133,#4133,#3510,.T.);
#5049=EDGE_CURVE('',#4133,#4134,#2618,.T.);
#5050=EDGE_CURVE('',#4134,#4134,#3511,.T.);
#5051=EDGE_CURVE('',#4135,#4135,#3512,.T.);
#5052=EDGE_CURVE('',#4135,#4136,#2619,.T.);
#5053=EDGE_CURVE('',#4136,#4136,#3513,.T.);
#5054=EDGE_CURVE('',#4137,#4137,#3514,.T.);
#5055=EDGE_CURVE('',#4137,#4138,#2620,.T.);
#5056=EDGE_CURVE('',#4138,#4138,#3515,.T.);
#5057=EDGE_CURVE('',#4139,#4139,#3516,.T.);
#5058=EDGE_CURVE('',#4139,#4140,#2621,.T.);
#5059=EDGE_CURVE('',#4140,#4140,#3517,.T.);
#5060=EDGE_CURVE('',#4141,#4142,#2622,.T.);
#5061=EDGE_CURVE('',#4141,#4142,#3518,.T.);
#5062=EDGE_CURVE('',#4143,#4141,#383,.T.);
#5063=EDGE_CURVE('',#4144,#4143,#3519,.T.);
#5064=EDGE_CURVE('',#4144,#4145,#2623,.T.);
#5065=EDGE_CURVE('',#4146,#4145,#384,.T.);
#5066=EDGE_CURVE('',#4145,#4146,#385,.T.);
#5067=EDGE_CURVE('',#4147,#4144,#3520,.T.);
#5068=EDGE_CURVE('',#4142,#4147,#386,.T.);
#5069=EDGE_CURVE('',#4147,#4143,#2624,.T.);
#5070=EDGE_CURVE('',#4148,#4148,#3521,.T.);
#5071=EDGE_CURVE('',#4148,#4149,#2625,.T.);
#5072=EDGE_CURVE('',#4149,#4149,#3522,.T.);
#5073=EDGE_CURVE('',#4150,#4150,#3523,.T.);
#5074=EDGE_CURVE('',#4150,#4151,#2626,.T.);
#5075=EDGE_CURVE('',#4151,#4151,#3524,.T.);
#5076=EDGE_CURVE('',#4152,#4153,#2627,.T.);
#5077=EDGE_CURVE('',#4152,#4153,#3525,.T.);
#5078=EDGE_CURVE('',#4154,#4152,#387,.T.);
#5079=EDGE_CURVE('',#4155,#4154,#3526,.T.);
#5080=EDGE_CURVE('',#4155,#4156,#2628,.T.);
#5081=EDGE_CURVE('',#4157,#4156,#388,.T.);
#5082=EDGE_CURVE('',#4156,#4157,#389,.T.);
#5083=EDGE_CURVE('',#4158,#4155,#3527,.T.);
#5084=EDGE_CURVE('',#4153,#4158,#390,.T.);
#5085=EDGE_CURVE('',#4158,#4154,#2629,.T.);
#5086=EDGE_CURVE('',#4159,#4159,#3528,.T.);
#5087=EDGE_CURVE('',#4159,#4160,#2630,.T.);
#5088=EDGE_CURVE('',#4160,#4160,#3529,.T.);
#5089=EDGE_CURVE('',#4161,#4161,#3530,.T.);
#5090=EDGE_CURVE('',#4161,#4162,#2631,.T.);
#5091=EDGE_CURVE('',#4162,#4162,#3531,.T.);
#5092=EDGE_CURVE('',#4163,#4164,#2632,.T.);
#5093=EDGE_CURVE('',#4163,#4164,#3532,.T.);
#5094=EDGE_CURVE('',#4165,#4163,#391,.T.);
#5095=EDGE_CURVE('',#4166,#4165,#3533,.T.);
#5096=EDGE_CURVE('',#4166,#4167,#2633,.T.);
#5097=EDGE_CURVE('',#4168,#4167,#392,.T.);
#5098=EDGE_CURVE('',#4167,#4168,#393,.T.);
#5099=EDGE_CURVE('',#4169,#4166,#3534,.T.);
#5100=EDGE_CURVE('',#4164,#4169,#394,.T.);
#5101=EDGE_CURVE('',#4169,#4165,#2634,.T.);
#5102=EDGE_CURVE('',#4170,#4170,#3535,.T.);
#5103=EDGE_CURVE('',#4170,#4171,#2635,.T.);
#5104=EDGE_CURVE('',#4171,#4171,#3536,.T.);
#5105=EDGE_CURVE('',#4172,#4172,#3537,.T.);
#5106=EDGE_CURVE('',#4172,#4173,#2636,.T.);
#5107=EDGE_CURVE('',#4173,#4173,#3538,.T.);
#5108=EDGE_CURVE('',#4174,#4174,#3539,.T.);
#5109=EDGE_CURVE('',#4174,#4175,#2637,.T.);
#5110=EDGE_CURVE('',#4175,#4175,#3540,.T.);
#5111=EDGE_CURVE('',#4176,#4176,#3541,.T.);
#5112=EDGE_CURVE('',#4176,#4177,#2638,.T.);
#5113=EDGE_CURVE('',#4177,#4177,#3542,.T.);
#5114=EDGE_CURVE('',#4178,#4178,#3543,.T.);
#5115=EDGE_CURVE('',#4179,#4179,#3544,.T.);
#5116=EDGE_CURVE('',#4178,#4180,#2639,.T.);
#5117=EDGE_CURVE('',#4180,#4180,#3545,.T.);
#5118=EDGE_CURVE('',#4181,#4181,#3546,.T.);
#5119=EDGE_CURVE('',#4181,#4182,#2640,.T.);
#5120=EDGE_CURVE('',#4182,#4182,#3547,.T.);
#5121=EDGE_CURVE('',#4183,#4183,#3548,.T.);
#5122=EDGE_CURVE('',#4183,#4179,#2641,.T.);
#5123=EDGE_CURVE('',#4184,#4185,#2642,.T.);
#5124=EDGE_CURVE('',#4184,#4186,#2643,.T.);
#5125=EDGE_CURVE('',#4186,#4187,#2644,.T.);
#5126=EDGE_CURVE('',#4185,#4187,#2645,.T.);
#5127=EDGE_CURVE('',#4188,#4184,#2646,.T.);
#5128=EDGE_CURVE('',#4188,#4189,#2647,.T.);
#5129=EDGE_CURVE('',#4189,#4186,#2648,.T.);
#5130=EDGE_CURVE('',#4190,#4188,#2649,.T.);
#5131=EDGE_CURVE('',#4190,#4191,#2650,.T.);
#5132=EDGE_CURVE('',#4191,#4189,#2651,.T.);
#5133=EDGE_CURVE('',#4192,#4190,#2652,.T.);
#5134=EDGE_CURVE('',#4192,#4193,#2653,.T.);
#5135=EDGE_CURVE('',#4193,#4191,#2654,.T.);
#5136=EDGE_CURVE('',#4194,#4192,#2655,.T.);
#5137=EDGE_CURVE('',#4194,#4195,#2656,.T.);
#5138=EDGE_CURVE('',#4195,#4193,#2657,.T.);
#5139=EDGE_CURVE('',#4185,#4194,#2658,.T.);
#5140=EDGE_CURVE('',#4187,#4195,#2659,.T.);
#5141=EDGE_CURVE('',#4196,#4196,#3549,.T.);
#5142=EDGE_CURVE('',#4197,#4197,#3550,.T.);
#5143=EDGE_CURVE('',#4197,#4196,#2660,.T.);
#5144=EDGE_CURVE('',#4198,#4198,#3551,.F.);
#5145=EDGE_CURVE('',#4198,#4197,#2661,.T.);
#5146=EDGE_CURVE('',#4199,#4199,#3552,.T.);
#5147=EDGE_CURVE('',#4199,#4198,#2662,.T.);
#5148=ORIENTED_EDGE('',*,*,#4200,.F.);
#5149=ORIENTED_EDGE('',*,*,#4201,.T.);
#5150=ORIENTED_EDGE('',*,*,#4202,.F.);
#5151=ORIENTED_EDGE('',*,*,#4201,.F.);
#5152=ORIENTED_EDGE('',*,*,#4203,.F.);
#5153=ORIENTED_EDGE('',*,*,#4204,.T.);
#5154=ORIENTED_EDGE('',*,*,#4205,.F.);
#5155=ORIENTED_EDGE('',*,*,#4204,.F.);
#5156=ORIENTED_EDGE('',*,*,#4206,.F.);
#5157=ORIENTED_EDGE('',*,*,#4207,.T.);
#5158=ORIENTED_EDGE('',*,*,#4208,.F.);
#5159=ORIENTED_EDGE('',*,*,#4207,.F.);
#5160=ORIENTED_EDGE('',*,*,#4209,.F.);
#5161=ORIENTED_EDGE('',*,*,#4210,.T.);
#5162=ORIENTED_EDGE('',*,*,#4211,.F.);
#5163=ORIENTED_EDGE('',*,*,#4210,.F.);
#5164=ORIENTED_EDGE('',*,*,#4212,.F.);
#5165=ORIENTED_EDGE('',*,*,#4213,.T.);
#5166=ORIENTED_EDGE('',*,*,#4214,.F.);
#5167=ORIENTED_EDGE('',*,*,#4213,.F.);
#5168=ORIENTED_EDGE('',*,*,#4215,.F.);
#5169=ORIENTED_EDGE('',*,*,#4216,.T.);
#5170=ORIENTED_EDGE('',*,*,#4217,.F.);
#5171=ORIENTED_EDGE('',*,*,#4216,.F.);
#5172=ORIENTED_EDGE('',*,*,#4218,.F.);
#5173=ORIENTED_EDGE('',*,*,#4219,.T.);
#5174=ORIENTED_EDGE('',*,*,#4220,.F.);
#5175=ORIENTED_EDGE('',*,*,#4219,.F.);
#5176=ORIENTED_EDGE('',*,*,#4221,.F.);
#5177=ORIENTED_EDGE('',*,*,#4222,.T.);
#5178=ORIENTED_EDGE('',*,*,#4223,.F.);
#5179=ORIENTED_EDGE('',*,*,#4222,.F.);
#5180=ORIENTED_EDGE('',*,*,#4224,.F.);
#5181=ORIENTED_EDGE('',*,*,#4225,.T.);
#5182=ORIENTED_EDGE('',*,*,#4226,.F.);
#5183=ORIENTED_EDGE('',*,*,#4225,.F.);
#5184=ORIENTED_EDGE('',*,*,#4227,.F.);
#5185=ORIENTED_EDGE('',*,*,#4228,.T.);
#5186=ORIENTED_EDGE('',*,*,#4229,.F.);
#5187=ORIENTED_EDGE('',*,*,#4228,.F.);
#5188=ORIENTED_EDGE('',*,*,#4230,.F.);
#5189=ORIENTED_EDGE('',*,*,#4231,.T.);
#5190=ORIENTED_EDGE('',*,*,#4232,.F.);
#5191=ORIENTED_EDGE('',*,*,#4231,.F.);
#5192=ORIENTED_EDGE('',*,*,#4233,.F.);
#5193=ORIENTED_EDGE('',*,*,#4234,.T.);
#5194=ORIENTED_EDGE('',*,*,#4235,.F.);
#5195=ORIENTED_EDGE('',*,*,#4234,.F.);
#5196=ORIENTED_EDGE('',*,*,#4236,.T.);
#5197=ORIENTED_EDGE('',*,*,#4237,.T.);
#5198=ORIENTED_EDGE('',*,*,#4238,.F.);
#5199=ORIENTED_EDGE('',*,*,#4239,.F.);
#5200=ORIENTED_EDGE('',*,*,#4240,.T.);
#5201=ORIENTED_EDGE('',*,*,#4239,.T.);
#5202=ORIENTED_EDGE('',*,*,#4241,.F.);
#5203=ORIENTED_EDGE('',*,*,#4242,.F.);
#5204=ORIENTED_EDGE('',*,*,#4243,.T.);
#5205=ORIENTED_EDGE('',*,*,#4242,.T.);
#5206=ORIENTED_EDGE('',*,*,#4244,.F.);
#5207=ORIENTED_EDGE('',*,*,#4245,.F.);
#5208=ORIENTED_EDGE('',*,*,#4246,.T.);
#5209=ORIENTED_EDGE('',*,*,#4245,.T.);
#5210=ORIENTED_EDGE('',*,*,#4247,.F.);
#5211=ORIENTED_EDGE('',*,*,#4237,.F.);
#5212=ORIENTED_EDGE('',*,*,#4247,.T.);
#5213=ORIENTED_EDGE('',*,*,#4244,.T.);
#5214=ORIENTED_EDGE('',*,*,#4241,.T.);
#5215=ORIENTED_EDGE('',*,*,#4238,.T.);
#5216=ORIENTED_EDGE('',*,*,#4205,.T.);
#5217=ORIENTED_EDGE('',*,*,#4211,.T.);
#5218=ORIENTED_EDGE('',*,*,#4235,.T.);
#5219=ORIENTED_EDGE('',*,*,#4232,.T.);
#5220=ORIENTED_EDGE('',*,*,#4229,.T.);
#5221=ORIENTED_EDGE('',*,*,#4226,.T.);
#5222=ORIENTED_EDGE('',*,*,#4223,.T.);
#5223=ORIENTED_EDGE('',*,*,#4220,.T.);
#5224=ORIENTED_EDGE('',*,*,#4217,.T.);
#5225=ORIENTED_EDGE('',*,*,#4214,.T.);
#5226=ORIENTED_EDGE('',*,*,#4208,.T.);
#5227=ORIENTED_EDGE('',*,*,#4202,.T.);
#5228=ORIENTED_EDGE('',*,*,#4246,.F.);
#5229=ORIENTED_EDGE('',*,*,#4236,.F.);
#5230=ORIENTED_EDGE('',*,*,#4240,.F.);
#5231=ORIENTED_EDGE('',*,*,#4243,.F.);
#5232=ORIENTED_EDGE('',*,*,#4203,.T.);
#5233=ORIENTED_EDGE('',*,*,#4209,.T.);
#5234=ORIENTED_EDGE('',*,*,#4233,.T.);
#5235=ORIENTED_EDGE('',*,*,#4230,.T.);
#5236=ORIENTED_EDGE('',*,*,#4227,.T.);
#5237=ORIENTED_EDGE('',*,*,#4224,.T.);
#5238=ORIENTED_EDGE('',*,*,#4221,.T.);
#5239=ORIENTED_EDGE('',*,*,#4218,.T.);
#5240=ORIENTED_EDGE('',*,*,#4215,.T.);
#5241=ORIENTED_EDGE('',*,*,#4212,.T.);
#5242=ORIENTED_EDGE('',*,*,#4206,.T.);
#5243=ORIENTED_EDGE('',*,*,#4200,.T.);
#5244=ORIENTED_EDGE('',*,*,#4248,.F.);
#5245=ORIENTED_EDGE('',*,*,#4249,.T.);
#5246=ORIENTED_EDGE('',*,*,#4250,.F.);
#5247=ORIENTED_EDGE('',*,*,#4249,.F.);
#5248=ORIENTED_EDGE('',*,*,#4251,.F.);
#5249=ORIENTED_EDGE('',*,*,#4252,.T.);
#5250=ORIENTED_EDGE('',*,*,#4253,.F.);
#5251=ORIENTED_EDGE('',*,*,#4252,.F.);
#5252=ORIENTED_EDGE('',*,*,#4254,.F.);
#5253=ORIENTED_EDGE('',*,*,#4255,.T.);
#5254=ORIENTED_EDGE('',*,*,#4256,.F.);
#5255=ORIENTED_EDGE('',*,*,#4255,.F.);
#5256=ORIENTED_EDGE('',*,*,#4257,.F.);
#5257=ORIENTED_EDGE('',*,*,#4258,.T.);
#5258=ORIENTED_EDGE('',*,*,#4259,.F.);
#5259=ORIENTED_EDGE('',*,*,#4258,.F.);
#5260=ORIENTED_EDGE('',*,*,#4260,.F.);
#5261=ORIENTED_EDGE('',*,*,#4261,.F.);
#5262=ORIENTED_EDGE('',*,*,#4262,.F.);
#5263=ORIENTED_EDGE('',*,*,#4263,.T.);
#5264=ORIENTED_EDGE('',*,*,#4264,.F.);
#5265=ORIENTED_EDGE('',*,*,#4261,.T.);
#5266=ORIENTED_EDGE('',*,*,#4265,.F.);
#5267=ORIENTED_EDGE('',*,*,#4263,.F.);
#5268=ORIENTED_EDGE('',*,*,#4262,.T.);
#5269=ORIENTED_EDGE('',*,*,#4266,.F.);
#5270=ORIENTED_EDGE('',*,*,#4267,.F.);
#5271=ORIENTED_EDGE('',*,*,#4268,.F.);
#5272=ORIENTED_EDGE('',*,*,#4269,.F.);
#5273=ORIENTED_EDGE('',*,*,#4270,.F.);
#5274=ORIENTED_EDGE('',*,*,#4271,.T.);
#5275=ORIENTED_EDGE('',*,*,#4268,.T.);
#5276=ORIENTED_EDGE('',*,*,#4272,.F.);
#5277=ORIENTED_EDGE('',*,*,#4269,.T.);
#5278=ORIENTED_EDGE('',*,*,#4271,.F.);
#5279=ORIENTED_EDGE('',*,*,#4270,.T.);
#5280=ORIENTED_EDGE('',*,*,#4273,.F.);
#5281=ORIENTED_EDGE('',*,*,#4274,.F.);
#5282=ORIENTED_EDGE('',*,*,#4275,.T.);
#5283=ORIENTED_EDGE('',*,*,#4266,.T.);
#5284=ORIENTED_EDGE('',*,*,#4275,.F.);
#5285=ORIENTED_EDGE('',*,*,#4276,.F.);
#5286=ORIENTED_EDGE('',*,*,#4277,.T.);
#5287=ORIENTED_EDGE('',*,*,#4273,.T.);
#5288=ORIENTED_EDGE('',*,*,#4277,.F.);
#5289=ORIENTED_EDGE('',*,*,#4278,.F.);
#5290=ORIENTED_EDGE('',*,*,#4279,.F.);
#5291=ORIENTED_EDGE('',*,*,#4280,.T.);
#5292=ORIENTED_EDGE('',*,*,#4281,.F.);
#5293=ORIENTED_EDGE('',*,*,#4272,.T.);
#5294=ORIENTED_EDGE('',*,*,#4267,.T.);
#5295=ORIENTED_EDGE('',*,*,#4282,.F.);
#5296=ORIENTED_EDGE('',*,*,#4283,.F.);
#5297=ORIENTED_EDGE('',*,*,#4284,.F.);
#5298=ORIENTED_EDGE('',*,*,#4285,.F.);
#5299=ORIENTED_EDGE('',*,*,#4264,.T.);
#5300=ORIENTED_EDGE('',*,*,#4265,.T.);
#5301=ORIENTED_EDGE('',*,*,#4260,.T.);
#5302=ORIENTED_EDGE('',*,*,#4286,.F.);
#5303=ORIENTED_EDGE('',*,*,#4284,.T.);
#5304=ORIENTED_EDGE('',*,*,#4287,.F.);
#5305=ORIENTED_EDGE('',*,*,#4288,.F.);
#5306=ORIENTED_EDGE('',*,*,#4289,.F.);
#5307=ORIENTED_EDGE('',*,*,#4288,.T.);
#5308=ORIENTED_EDGE('',*,*,#4290,.F.);
#5309=ORIENTED_EDGE('',*,*,#4291,.F.);
#5310=ORIENTED_EDGE('',*,*,#4274,.T.);
#5311=ORIENTED_EDGE('',*,*,#4276,.T.);
#5312=ORIENTED_EDGE('',*,*,#4292,.F.);
#5313=ORIENTED_EDGE('',*,*,#4291,.T.);
#5314=ORIENTED_EDGE('',*,*,#4293,.F.);
#5315=ORIENTED_EDGE('',*,*,#4280,.F.);
#5316=ORIENTED_EDGE('',*,*,#4294,.T.);
#5317=ORIENTED_EDGE('',*,*,#4281,.T.);
#5318=ORIENTED_EDGE('',*,*,#4293,.T.);
#5319=ORIENTED_EDGE('',*,*,#4290,.T.);
#5320=ORIENTED_EDGE('',*,*,#4287,.T.);
#5321=ORIENTED_EDGE('',*,*,#4283,.T.);
#5322=ORIENTED_EDGE('',*,*,#4295,.T.);
#5323=ORIENTED_EDGE('',*,*,#4259,.T.);
#5324=ORIENTED_EDGE('',*,*,#4256,.T.);
#5325=ORIENTED_EDGE('',*,*,#4253,.T.);
#5326=ORIENTED_EDGE('',*,*,#4250,.T.);
#5327=ORIENTED_EDGE('',*,*,#4295,.F.);
#5328=ORIENTED_EDGE('',*,*,#4296,.T.);
#5329=ORIENTED_EDGE('',*,*,#4297,.T.);
#5330=ORIENTED_EDGE('',*,*,#4296,.F.);
#5331=ORIENTED_EDGE('',*,*,#4278,.T.);
#5332=ORIENTED_EDGE('',*,*,#4294,.F.);
#5333=ORIENTED_EDGE('',*,*,#4282,.T.);
#5334=ORIENTED_EDGE('',*,*,#4298,.T.);
#5335=ORIENTED_EDGE('',*,*,#4298,.F.);
#5336=ORIENTED_EDGE('',*,*,#4285,.T.);
#5337=ORIENTED_EDGE('',*,*,#4286,.T.);
#5338=ORIENTED_EDGE('',*,*,#4289,.T.);
#5339=ORIENTED_EDGE('',*,*,#4292,.T.);
#5340=ORIENTED_EDGE('',*,*,#4279,.T.);
#5341=ORIENTED_EDGE('',*,*,#4297,.F.);
#5342=ORIENTED_EDGE('',*,*,#4257,.T.);
#5343=ORIENTED_EDGE('',*,*,#4254,.T.);
#5344=ORIENTED_EDGE('',*,*,#4251,.T.);
#5345=ORIENTED_EDGE('',*,*,#4248,.T.);
#5346=ORIENTED_EDGE('',*,*,#4299,.F.);
#5347=ORIENTED_EDGE('',*,*,#4300,.T.);
#5348=ORIENTED_EDGE('',*,*,#4301,.F.);
#5349=ORIENTED_EDGE('',*,*,#4300,.F.);
#5350=ORIENTED_EDGE('',*,*,#4302,.F.);
#5351=ORIENTED_EDGE('',*,*,#4303,.T.);
#5352=ORIENTED_EDGE('',*,*,#4304,.F.);
#5353=ORIENTED_EDGE('',*,*,#4303,.F.);
#5354=ORIENTED_EDGE('',*,*,#4305,.F.);
#5355=ORIENTED_EDGE('',*,*,#4306,.T.);
#5356=ORIENTED_EDGE('',*,*,#4307,.F.);
#5357=ORIENTED_EDGE('',*,*,#4306,.F.);
#5358=ORIENTED_EDGE('',*,*,#4308,.F.);
#5359=ORIENTED_EDGE('',*,*,#4309,.T.);
#5360=ORIENTED_EDGE('',*,*,#4310,.F.);
#5361=ORIENTED_EDGE('',*,*,#4309,.F.);
#5362=ORIENTED_EDGE('',*,*,#4311,.F.);
#5363=ORIENTED_EDGE('',*,*,#4312,.T.);
#5364=ORIENTED_EDGE('',*,*,#4313,.F.);
#5365=ORIENTED_EDGE('',*,*,#4312,.F.);
#5366=ORIENTED_EDGE('',*,*,#4311,.T.);
#5367=ORIENTED_EDGE('',*,*,#4314,.T.);
#5368=ORIENTED_EDGE('',*,*,#4314,.F.);
#5369=ORIENTED_EDGE('',*,*,#4315,.T.);
#5370=ORIENTED_EDGE('',*,*,#4316,.T.);
#5371=ORIENTED_EDGE('',*,*,#4315,.F.);
#5372=ORIENTED_EDGE('',*,*,#4317,.F.);
#5373=ORIENTED_EDGE('',*,*,#4318,.T.);
#5374=ORIENTED_EDGE('',*,*,#4319,.T.);
#5375=ORIENTED_EDGE('',*,*,#4318,.F.);
#5376=ORIENTED_EDGE('',*,*,#4317,.T.);
#5377=ORIENTED_EDGE('',*,*,#4313,.T.);
#5378=ORIENTED_EDGE('',*,*,#4310,.T.);
#5379=ORIENTED_EDGE('',*,*,#4307,.T.);
#5380=ORIENTED_EDGE('',*,*,#4304,.T.);
#5381=ORIENTED_EDGE('',*,*,#4301,.T.);
#5382=ORIENTED_EDGE('',*,*,#4319,.F.);
#5383=ORIENTED_EDGE('',*,*,#4316,.F.);
#5384=ORIENTED_EDGE('',*,*,#4308,.T.);
#5385=ORIENTED_EDGE('',*,*,#4305,.T.);
#5386=ORIENTED_EDGE('',*,*,#4302,.T.);
#5387=ORIENTED_EDGE('',*,*,#4299,.T.);
#5388=ORIENTED_EDGE('',*,*,#4320,.F.);
#5389=ORIENTED_EDGE('',*,*,#4321,.T.);
#5390=ORIENTED_EDGE('',*,*,#4322,.F.);
#5391=ORIENTED_EDGE('',*,*,#4321,.F.);
#5392=ORIENTED_EDGE('',*,*,#4323,.F.);
#5393=ORIENTED_EDGE('',*,*,#4324,.T.);
#5394=ORIENTED_EDGE('',*,*,#4325,.F.);
#5395=ORIENTED_EDGE('',*,*,#4324,.F.);
#5396=ORIENTED_EDGE('',*,*,#4326,.F.);
#5397=ORIENTED_EDGE('',*,*,#4327,.T.);
#5398=ORIENTED_EDGE('',*,*,#4328,.F.);
#5399=ORIENTED_EDGE('',*,*,#4327,.F.);
#5400=ORIENTED_EDGE('',*,*,#4329,.F.);
#5401=ORIENTED_EDGE('',*,*,#4330,.T.);
#5402=ORIENTED_EDGE('',*,*,#4331,.F.);
#5403=ORIENTED_EDGE('',*,*,#4330,.F.);
#5404=ORIENTED_EDGE('',*,*,#4332,.F.);
#5405=ORIENTED_EDGE('',*,*,#4333,.T.);
#5406=ORIENTED_EDGE('',*,*,#4334,.T.);
#5407=ORIENTED_EDGE('',*,*,#4333,.F.);
#5408=ORIENTED_EDGE('',*,*,#4334,.F.);
#5409=ORIENTED_EDGE('',*,*,#4335,.F.);
#5410=ORIENTED_EDGE('',*,*,#4336,.F.);
#5411=ORIENTED_EDGE('',*,*,#4337,.T.);
#5412=ORIENTED_EDGE('',*,*,#4335,.T.);
#5413=ORIENTED_EDGE('',*,*,#4337,.F.);
#5414=ORIENTED_EDGE('',*,*,#4338,.F.);
#5415=ORIENTED_EDGE('',*,*,#4339,.T.);
#5416=ORIENTED_EDGE('',*,*,#4340,.T.);
#5417=ORIENTED_EDGE('',*,*,#4339,.F.);
#5418=ORIENTED_EDGE('',*,*,#4338,.T.);
#5419=ORIENTED_EDGE('',*,*,#4336,.T.);
#5420=ORIENTED_EDGE('',*,*,#4331,.T.);
#5421=ORIENTED_EDGE('',*,*,#4328,.T.);
#5422=ORIENTED_EDGE('',*,*,#4325,.T.);
#5423=ORIENTED_EDGE('',*,*,#4322,.T.);
#5424=ORIENTED_EDGE('',*,*,#4340,.F.);
#5425=ORIENTED_EDGE('',*,*,#4332,.T.);
#5426=ORIENTED_EDGE('',*,*,#4329,.T.);
#5427=ORIENTED_EDGE('',*,*,#4326,.T.);
#5428=ORIENTED_EDGE('',*,*,#4323,.T.);
#5429=ORIENTED_EDGE('',*,*,#4320,.T.);
#5430=ORIENTED_EDGE('',*,*,#4341,.F.);
#5431=ORIENTED_EDGE('',*,*,#4342,.T.);
#5432=ORIENTED_EDGE('',*,*,#4343,.F.);
#5433=ORIENTED_EDGE('',*,*,#4342,.F.);
#5434=ORIENTED_EDGE('',*,*,#4344,.F.);
#5435=ORIENTED_EDGE('',*,*,#4345,.T.);
#5436=ORIENTED_EDGE('',*,*,#4346,.F.);
#5437=ORIENTED_EDGE('',*,*,#4345,.F.);
#5438=ORIENTED_EDGE('',*,*,#4347,.F.);
#5439=ORIENTED_EDGE('',*,*,#4348,.T.);
#5440=ORIENTED_EDGE('',*,*,#4349,.F.);
#5441=ORIENTED_EDGE('',*,*,#4348,.F.);
#5442=ORIENTED_EDGE('',*,*,#4350,.F.);
#5443=ORIENTED_EDGE('',*,*,#4351,.T.);
#5444=ORIENTED_EDGE('',*,*,#4352,.F.);
#5445=ORIENTED_EDGE('',*,*,#4351,.F.);
#5446=ORIENTED_EDGE('',*,*,#4353,.F.);
#5447=ORIENTED_EDGE('',*,*,#4354,.F.);
#5448=ORIENTED_EDGE('',*,*,#4355,.F.);
#5449=ORIENTED_EDGE('',*,*,#4356,.T.);
#5450=ORIENTED_EDGE('',*,*,#4357,.F.);
#5451=ORIENTED_EDGE('',*,*,#4354,.T.);
#5452=ORIENTED_EDGE('',*,*,#4358,.F.);
#5453=ORIENTED_EDGE('',*,*,#4356,.F.);
#5454=ORIENTED_EDGE('',*,*,#4355,.T.);
#5455=ORIENTED_EDGE('',*,*,#4359,.F.);
#5456=ORIENTED_EDGE('',*,*,#4360,.F.);
#5457=ORIENTED_EDGE('',*,*,#4361,.F.);
#5458=ORIENTED_EDGE('',*,*,#4362,.F.);
#5459=ORIENTED_EDGE('',*,*,#4363,.F.);
#5460=ORIENTED_EDGE('',*,*,#4364,.T.);
#5461=ORIENTED_EDGE('',*,*,#4361,.T.);
#5462=ORIENTED_EDGE('',*,*,#4365,.F.);
#5463=ORIENTED_EDGE('',*,*,#4362,.T.);
#5464=ORIENTED_EDGE('',*,*,#4364,.F.);
#5465=ORIENTED_EDGE('',*,*,#4363,.T.);
#5466=ORIENTED_EDGE('',*,*,#4366,.F.);
#5467=ORIENTED_EDGE('',*,*,#4367,.F.);
#5468=ORIENTED_EDGE('',*,*,#4368,.T.);
#5469=ORIENTED_EDGE('',*,*,#4359,.T.);
#5470=ORIENTED_EDGE('',*,*,#4368,.F.);
#5471=ORIENTED_EDGE('',*,*,#4369,.F.);
#5472=ORIENTED_EDGE('',*,*,#4370,.T.);
#5473=ORIENTED_EDGE('',*,*,#4366,.T.);
#5474=ORIENTED_EDGE('',*,*,#4370,.F.);
#5475=ORIENTED_EDGE('',*,*,#4371,.F.);
#5476=ORIENTED_EDGE('',*,*,#4372,.F.);
#5477=ORIENTED_EDGE('',*,*,#4373,.T.);
#5478=ORIENTED_EDGE('',*,*,#4374,.F.);
#5479=ORIENTED_EDGE('',*,*,#4365,.T.);
#5480=ORIENTED_EDGE('',*,*,#4360,.T.);
#5481=ORIENTED_EDGE('',*,*,#4375,.F.);
#5482=ORIENTED_EDGE('',*,*,#4376,.F.);
#5483=ORIENTED_EDGE('',*,*,#4377,.F.);
#5484=ORIENTED_EDGE('',*,*,#4378,.F.);
#5485=ORIENTED_EDGE('',*,*,#4357,.T.);
#5486=ORIENTED_EDGE('',*,*,#4358,.T.);
#5487=ORIENTED_EDGE('',*,*,#4353,.T.);
#5488=ORIENTED_EDGE('',*,*,#4379,.F.);
#5489=ORIENTED_EDGE('',*,*,#4377,.T.);
#5490=ORIENTED_EDGE('',*,*,#4380,.F.);
#5491=ORIENTED_EDGE('',*,*,#4381,.F.);
#5492=ORIENTED_EDGE('',*,*,#4382,.F.);
#5493=ORIENTED_EDGE('',*,*,#4381,.T.);
#5494=ORIENTED_EDGE('',*,*,#4383,.F.);
#5495=ORIENTED_EDGE('',*,*,#4384,.F.);
#5496=ORIENTED_EDGE('',*,*,#4367,.T.);
#5497=ORIENTED_EDGE('',*,*,#4369,.T.);
#5498=ORIENTED_EDGE('',*,*,#4385,.F.);
#5499=ORIENTED_EDGE('',*,*,#4384,.T.);
#5500=ORIENTED_EDGE('',*,*,#4386,.F.);
#5501=ORIENTED_EDGE('',*,*,#4373,.F.);
#5502=ORIENTED_EDGE('',*,*,#4387,.T.);
#5503=ORIENTED_EDGE('',*,*,#4374,.T.);
#5504=ORIENTED_EDGE('',*,*,#4386,.T.);
#5505=ORIENTED_EDGE('',*,*,#4383,.T.);
#5506=ORIENTED_EDGE('',*,*,#4380,.T.);
#5507=ORIENTED_EDGE('',*,*,#4376,.T.);
#5508=ORIENTED_EDGE('',*,*,#4388,.T.);
#5509=ORIENTED_EDGE('',*,*,#4352,.T.);
#5510=ORIENTED_EDGE('',*,*,#4349,.T.);
#5511=ORIENTED_EDGE('',*,*,#4346,.T.);
#5512=ORIENTED_EDGE('',*,*,#4343,.T.);
#5513=ORIENTED_EDGE('',*,*,#4388,.F.);
#5514=ORIENTED_EDGE('',*,*,#4389,.T.);
#5515=ORIENTED_EDGE('',*,*,#4390,.T.);
#5516=ORIENTED_EDGE('',*,*,#4389,.F.);
#5517=ORIENTED_EDGE('',*,*,#4371,.T.);
#5518=ORIENTED_EDGE('',*,*,#4387,.F.);
#5519=ORIENTED_EDGE('',*,*,#4375,.T.);
#5520=ORIENTED_EDGE('',*,*,#4391,.T.);
#5521=ORIENTED_EDGE('',*,*,#4391,.F.);
#5522=ORIENTED_EDGE('',*,*,#4378,.T.);
#5523=ORIENTED_EDGE('',*,*,#4379,.T.);
#5524=ORIENTED_EDGE('',*,*,#4382,.T.);
#5525=ORIENTED_EDGE('',*,*,#4385,.T.);
#5526=ORIENTED_EDGE('',*,*,#4372,.T.);
#5527=ORIENTED_EDGE('',*,*,#4390,.F.);
#5528=ORIENTED_EDGE('',*,*,#4350,.T.);
#5529=ORIENTED_EDGE('',*,*,#4347,.T.);
#5530=ORIENTED_EDGE('',*,*,#4344,.T.);
#5531=ORIENTED_EDGE('',*,*,#4341,.T.);
#5532=ORIENTED_EDGE('',*,*,#4392,.F.);
#5533=ORIENTED_EDGE('',*,*,#4393,.T.);
#5534=ORIENTED_EDGE('',*,*,#4394,.F.);
#5535=ORIENTED_EDGE('',*,*,#4393,.F.);
#5536=ORIENTED_EDGE('',*,*,#4395,.F.);
#5537=ORIENTED_EDGE('',*,*,#4396,.T.);
#5538=ORIENTED_EDGE('',*,*,#4397,.F.);
#5539=ORIENTED_EDGE('',*,*,#4396,.F.);
#5540=ORIENTED_EDGE('',*,*,#4398,.F.);
#5541=ORIENTED_EDGE('',*,*,#4399,.T.);
#5542=ORIENTED_EDGE('',*,*,#4400,.F.);
#5543=ORIENTED_EDGE('',*,*,#4399,.F.);
#5544=ORIENTED_EDGE('',*,*,#4401,.F.);
#5545=ORIENTED_EDGE('',*,*,#4402,.T.);
#5546=ORIENTED_EDGE('',*,*,#4403,.F.);
#5547=ORIENTED_EDGE('',*,*,#4402,.F.);
#5548=ORIENTED_EDGE('',*,*,#4404,.F.);
#5549=ORIENTED_EDGE('',*,*,#4405,.T.);
#5550=ORIENTED_EDGE('',*,*,#4406,.F.);
#5551=ORIENTED_EDGE('',*,*,#4405,.F.);
#5552=ORIENTED_EDGE('',*,*,#4404,.T.);
#5553=ORIENTED_EDGE('',*,*,#4407,.T.);
#5554=ORIENTED_EDGE('',*,*,#4407,.F.);
#5555=ORIENTED_EDGE('',*,*,#4408,.T.);
#5556=ORIENTED_EDGE('',*,*,#4409,.T.);
#5557=ORIENTED_EDGE('',*,*,#4408,.F.);
#5558=ORIENTED_EDGE('',*,*,#4410,.F.);
#5559=ORIENTED_EDGE('',*,*,#4411,.T.);
#5560=ORIENTED_EDGE('',*,*,#4412,.T.);
#5561=ORIENTED_EDGE('',*,*,#4411,.F.);
#5562=ORIENTED_EDGE('',*,*,#4410,.T.);
#5563=ORIENTED_EDGE('',*,*,#4406,.T.);
#5564=ORIENTED_EDGE('',*,*,#4403,.T.);
#5565=ORIENTED_EDGE('',*,*,#4400,.T.);
#5566=ORIENTED_EDGE('',*,*,#4397,.T.);
#5567=ORIENTED_EDGE('',*,*,#4394,.T.);
#5568=ORIENTED_EDGE('',*,*,#4412,.F.);
#5569=ORIENTED_EDGE('',*,*,#4409,.F.);
#5570=ORIENTED_EDGE('',*,*,#4401,.T.);
#5571=ORIENTED_EDGE('',*,*,#4398,.T.);
#5572=ORIENTED_EDGE('',*,*,#4395,.T.);
#5573=ORIENTED_EDGE('',*,*,#4392,.T.);
#5574=ORIENTED_EDGE('',*,*,#4413,.F.);
#5575=ORIENTED_EDGE('',*,*,#4414,.T.);
#5576=ORIENTED_EDGE('',*,*,#4415,.F.);
#5577=ORIENTED_EDGE('',*,*,#4414,.F.);
#5578=ORIENTED_EDGE('',*,*,#4416,.F.);
#5579=ORIENTED_EDGE('',*,*,#4417,.T.);
#5580=ORIENTED_EDGE('',*,*,#4418,.F.);
#5581=ORIENTED_EDGE('',*,*,#4417,.F.);
#5582=ORIENTED_EDGE('',*,*,#4419,.F.);
#5583=ORIENTED_EDGE('',*,*,#4420,.T.);
#5584=ORIENTED_EDGE('',*,*,#4421,.F.);
#5585=ORIENTED_EDGE('',*,*,#4420,.F.);
#5586=ORIENTED_EDGE('',*,*,#4422,.F.);
#5587=ORIENTED_EDGE('',*,*,#4423,.T.);
#5588=ORIENTED_EDGE('',*,*,#4424,.F.);
#5589=ORIENTED_EDGE('',*,*,#4423,.F.);
#5590=ORIENTED_EDGE('',*,*,#4425,.F.);
#5591=ORIENTED_EDGE('',*,*,#4426,.T.);
#5592=ORIENTED_EDGE('',*,*,#4427,.T.);
#5593=ORIENTED_EDGE('',*,*,#4426,.F.);
#5594=ORIENTED_EDGE('',*,*,#4427,.F.);
#5595=ORIENTED_EDGE('',*,*,#4428,.F.);
#5596=ORIENTED_EDGE('',*,*,#4429,.F.);
#5597=ORIENTED_EDGE('',*,*,#4430,.T.);
#5598=ORIENTED_EDGE('',*,*,#4428,.T.);
#5599=ORIENTED_EDGE('',*,*,#4430,.F.);
#5600=ORIENTED_EDGE('',*,*,#4431,.F.);
#5601=ORIENTED_EDGE('',*,*,#4432,.T.);
#5602=ORIENTED_EDGE('',*,*,#4433,.T.);
#5603=ORIENTED_EDGE('',*,*,#4432,.F.);
#5604=ORIENTED_EDGE('',*,*,#4431,.T.);
#5605=ORIENTED_EDGE('',*,*,#4429,.T.);
#5606=ORIENTED_EDGE('',*,*,#4424,.T.);
#5607=ORIENTED_EDGE('',*,*,#4421,.T.);
#5608=ORIENTED_EDGE('',*,*,#4418,.T.);
#5609=ORIENTED_EDGE('',*,*,#4415,.T.);
#5610=ORIENTED_EDGE('',*,*,#4433,.F.);
#5611=ORIENTED_EDGE('',*,*,#4425,.T.);
#5612=ORIENTED_EDGE('',*,*,#4422,.T.);
#5613=ORIENTED_EDGE('',*,*,#4419,.T.);
#5614=ORIENTED_EDGE('',*,*,#4416,.T.);
#5615=ORIENTED_EDGE('',*,*,#4413,.T.);
#5616=ORIENTED_EDGE('',*,*,#4434,.F.);
#5617=ORIENTED_EDGE('',*,*,#4435,.T.);
#5618=ORIENTED_EDGE('',*,*,#4436,.F.);
#5619=ORIENTED_EDGE('',*,*,#4435,.F.);
#5620=ORIENTED_EDGE('',*,*,#4437,.F.);
#5621=ORIENTED_EDGE('',*,*,#4438,.T.);
#5622=ORIENTED_EDGE('',*,*,#4439,.F.);
#5623=ORIENTED_EDGE('',*,*,#4438,.F.);
#5624=ORIENTED_EDGE('',*,*,#4440,.F.);
#5625=ORIENTED_EDGE('',*,*,#4441,.T.);
#5626=ORIENTED_EDGE('',*,*,#4442,.F.);
#5627=ORIENTED_EDGE('',*,*,#4441,.F.);
#5628=ORIENTED_EDGE('',*,*,#4443,.F.);
#5629=ORIENTED_EDGE('',*,*,#4444,.T.);
#5630=ORIENTED_EDGE('',*,*,#4445,.F.);
#5631=ORIENTED_EDGE('',*,*,#4444,.F.);
#5632=ORIENTED_EDGE('',*,*,#4446,.F.);
#5633=ORIENTED_EDGE('',*,*,#4447,.F.);
#5634=ORIENTED_EDGE('',*,*,#4448,.F.);
#5635=ORIENTED_EDGE('',*,*,#4449,.F.);
#5636=ORIENTED_EDGE('',*,*,#4450,.F.);
#5637=ORIENTED_EDGE('',*,*,#4451,.T.);
#5638=ORIENTED_EDGE('',*,*,#4452,.T.);
#5639=ORIENTED_EDGE('',*,*,#4447,.T.);
#5640=ORIENTED_EDGE('',*,*,#4453,.F.);
#5641=ORIENTED_EDGE('',*,*,#4449,.T.);
#5642=ORIENTED_EDGE('',*,*,#4454,.T.);
#5643=ORIENTED_EDGE('',*,*,#4455,.T.);
#5644=ORIENTED_EDGE('',*,*,#4456,.F.);
#5645=ORIENTED_EDGE('',*,*,#4455,.F.);
#5646=ORIENTED_EDGE('',*,*,#4457,.T.);
#5647=ORIENTED_EDGE('',*,*,#4451,.F.);
#5648=ORIENTED_EDGE('',*,*,#4454,.F.);
#5649=ORIENTED_EDGE('',*,*,#4448,.T.);
#5650=ORIENTED_EDGE('',*,*,#4452,.F.);
#5651=ORIENTED_EDGE('',*,*,#4457,.F.);
#5652=ORIENTED_EDGE('',*,*,#4458,.F.);
#5653=ORIENTED_EDGE('',*,*,#4459,.T.);
#5654=ORIENTED_EDGE('',*,*,#4460,.T.);
#5655=ORIENTED_EDGE('',*,*,#4459,.F.);
#5656=ORIENTED_EDGE('',*,*,#4461,.F.);
#5657=ORIENTED_EDGE('',*,*,#4462,.T.);
#5658=ORIENTED_EDGE('',*,*,#4463,.T.);
#5659=ORIENTED_EDGE('',*,*,#4462,.F.);
#5660=ORIENTED_EDGE('',*,*,#4456,.T.);
#5661=ORIENTED_EDGE('',*,*,#4450,.T.);
#5662=ORIENTED_EDGE('',*,*,#4446,.T.);
#5663=ORIENTED_EDGE('',*,*,#4453,.T.);
#5664=ORIENTED_EDGE('',*,*,#4461,.T.);
#5665=ORIENTED_EDGE('',*,*,#4458,.T.);
#5666=ORIENTED_EDGE('',*,*,#4445,.T.);
#5667=ORIENTED_EDGE('',*,*,#4442,.T.);
#5668=ORIENTED_EDGE('',*,*,#4439,.T.);
#5669=ORIENTED_EDGE('',*,*,#4436,.T.);
#5670=ORIENTED_EDGE('',*,*,#4463,.F.);
#5671=ORIENTED_EDGE('',*,*,#4460,.F.);
#5672=ORIENTED_EDGE('',*,*,#4443,.T.);
#5673=ORIENTED_EDGE('',*,*,#4440,.T.);
#5674=ORIENTED_EDGE('',*,*,#4437,.T.);
#5675=ORIENTED_EDGE('',*,*,#4434,.T.);
#5676=ORIENTED_EDGE('',*,*,#4464,.F.);
#5677=ORIENTED_EDGE('',*,*,#4465,.T.);
#5678=ORIENTED_EDGE('',*,*,#4466,.F.);
#5679=ORIENTED_EDGE('',*,*,#4465,.F.);
#5680=ORIENTED_EDGE('',*,*,#4467,.F.);
#5681=ORIENTED_EDGE('',*,*,#4468,.T.);
#5682=ORIENTED_EDGE('',*,*,#4469,.F.);
#5683=ORIENTED_EDGE('',*,*,#4468,.F.);
#5684=ORIENTED_EDGE('',*,*,#4470,.F.);
#5685=ORIENTED_EDGE('',*,*,#4471,.T.);
#5686=ORIENTED_EDGE('',*,*,#4472,.F.);
#5687=ORIENTED_EDGE('',*,*,#4471,.F.);
#5688=ORIENTED_EDGE('',*,*,#4473,.F.);
#5689=ORIENTED_EDGE('',*,*,#4474,.T.);
#5690=ORIENTED_EDGE('',*,*,#4475,.F.);
#5691=ORIENTED_EDGE('',*,*,#4474,.F.);
#5692=ORIENTED_EDGE('',*,*,#4476,.F.);
#5693=ORIENTED_EDGE('',*,*,#4477,.T.);
#5694=ORIENTED_EDGE('',*,*,#4478,.F.);
#5695=ORIENTED_EDGE('',*,*,#4477,.F.);
#5696=ORIENTED_EDGE('',*,*,#4476,.T.);
#5697=ORIENTED_EDGE('',*,*,#4479,.T.);
#5698=ORIENTED_EDGE('',*,*,#4479,.F.);
#5699=ORIENTED_EDGE('',*,*,#4480,.T.);
#5700=ORIENTED_EDGE('',*,*,#4481,.T.);
#5701=ORIENTED_EDGE('',*,*,#4480,.F.);
#5702=ORIENTED_EDGE('',*,*,#4482,.F.);
#5703=ORIENTED_EDGE('',*,*,#4483,.T.);
#5704=ORIENTED_EDGE('',*,*,#4484,.T.);
#5705=ORIENTED_EDGE('',*,*,#4483,.F.);
#5706=ORIENTED_EDGE('',*,*,#4482,.T.);
#5707=ORIENTED_EDGE('',*,*,#4478,.T.);
#5708=ORIENTED_EDGE('',*,*,#4475,.T.);
#5709=ORIENTED_EDGE('',*,*,#4472,.T.);
#5710=ORIENTED_EDGE('',*,*,#4469,.T.);
#5711=ORIENTED_EDGE('',*,*,#4466,.T.);
#5712=ORIENTED_EDGE('',*,*,#4484,.F.);
#5713=ORIENTED_EDGE('',*,*,#4481,.F.);
#5714=ORIENTED_EDGE('',*,*,#4473,.T.);
#5715=ORIENTED_EDGE('',*,*,#4470,.T.);
#5716=ORIENTED_EDGE('',*,*,#4467,.T.);
#5717=ORIENTED_EDGE('',*,*,#4464,.T.);
#5718=ORIENTED_EDGE('',*,*,#4485,.F.);
#5719=ORIENTED_EDGE('',*,*,#4486,.T.);
#5720=ORIENTED_EDGE('',*,*,#4487,.F.);
#5721=ORIENTED_EDGE('',*,*,#4486,.F.);
#5722=ORIENTED_EDGE('',*,*,#4488,.F.);
#5723=ORIENTED_EDGE('',*,*,#4489,.T.);
#5724=ORIENTED_EDGE('',*,*,#4490,.F.);
#5725=ORIENTED_EDGE('',*,*,#4489,.F.);
#5726=ORIENTED_EDGE('',*,*,#4491,.F.);
#5727=ORIENTED_EDGE('',*,*,#4492,.T.);
#5728=ORIENTED_EDGE('',*,*,#4493,.F.);
#5729=ORIENTED_EDGE('',*,*,#4492,.F.);
#5730=ORIENTED_EDGE('',*,*,#4494,.F.);
#5731=ORIENTED_EDGE('',*,*,#4495,.T.);
#5732=ORIENTED_EDGE('',*,*,#4496,.F.);
#5733=ORIENTED_EDGE('',*,*,#4495,.F.);
#5734=ORIENTED_EDGE('',*,*,#4497,.F.);
#5735=ORIENTED_EDGE('',*,*,#4498,.T.);
#5736=ORIENTED_EDGE('',*,*,#4499,.T.);
#5737=ORIENTED_EDGE('',*,*,#4498,.F.);
#5738=ORIENTED_EDGE('',*,*,#4499,.F.);
#5739=ORIENTED_EDGE('',*,*,#4500,.F.);
#5740=ORIENTED_EDGE('',*,*,#4501,.F.);
#5741=ORIENTED_EDGE('',*,*,#4502,.T.);
#5742=ORIENTED_EDGE('',*,*,#4500,.T.);
#5743=ORIENTED_EDGE('',*,*,#4502,.F.);
#5744=ORIENTED_EDGE('',*,*,#4503,.F.);
#5745=ORIENTED_EDGE('',*,*,#4504,.T.);
#5746=ORIENTED_EDGE('',*,*,#4505,.T.);
#5747=ORIENTED_EDGE('',*,*,#4504,.F.);
#5748=ORIENTED_EDGE('',*,*,#4503,.T.);
#5749=ORIENTED_EDGE('',*,*,#4501,.T.);
#5750=ORIENTED_EDGE('',*,*,#4496,.T.);
#5751=ORIENTED_EDGE('',*,*,#4493,.T.);
#5752=ORIENTED_EDGE('',*,*,#4490,.T.);
#5753=ORIENTED_EDGE('',*,*,#4487,.T.);
#5754=ORIENTED_EDGE('',*,*,#4505,.F.);
#5755=ORIENTED_EDGE('',*,*,#4497,.T.);
#5756=ORIENTED_EDGE('',*,*,#4494,.T.);
#5757=ORIENTED_EDGE('',*,*,#4491,.T.);
#5758=ORIENTED_EDGE('',*,*,#4488,.T.);
#5759=ORIENTED_EDGE('',*,*,#4485,.T.);
#5760=ORIENTED_EDGE('',*,*,#4506,.F.);
#5761=ORIENTED_EDGE('',*,*,#4507,.T.);
#5762=ORIENTED_EDGE('',*,*,#4508,.F.);
#5763=ORIENTED_EDGE('',*,*,#4507,.F.);
#5764=ORIENTED_EDGE('',*,*,#4506,.T.);
#5765=ORIENTED_EDGE('',*,*,#4509,.F.);
#5766=ORIENTED_EDGE('',*,*,#4510,.T.);
#5767=ORIENTED_EDGE('',*,*,#4511,.F.);
#5768=ORIENTED_EDGE('',*,*,#4510,.F.);
#5769=ORIENTED_EDGE('',*,*,#4509,.T.);
#5770=ORIENTED_EDGE('',*,*,#4512,.F.);
#5771=ORIENTED_EDGE('',*,*,#4513,.T.);
#5772=ORIENTED_EDGE('',*,*,#4514,.F.);
#5773=ORIENTED_EDGE('',*,*,#4513,.F.);
#5774=ORIENTED_EDGE('',*,*,#4512,.T.);
#5775=ORIENTED_EDGE('',*,*,#4515,.F.);
#5776=ORIENTED_EDGE('',*,*,#4516,.F.);
#5777=ORIENTED_EDGE('',*,*,#4517,.T.);
#5778=ORIENTED_EDGE('',*,*,#4518,.F.);
#5779=ORIENTED_EDGE('',*,*,#4517,.F.);
#5780=ORIENTED_EDGE('',*,*,#4516,.T.);
#5781=ORIENTED_EDGE('',*,*,#4519,.F.);
#5782=ORIENTED_EDGE('',*,*,#4520,.F.);
#5783=ORIENTED_EDGE('',*,*,#4521,.T.);
#5784=ORIENTED_EDGE('',*,*,#4522,.F.);
#5785=ORIENTED_EDGE('',*,*,#4521,.F.);
#5786=ORIENTED_EDGE('',*,*,#4520,.T.);
#5787=ORIENTED_EDGE('',*,*,#4523,.F.);
#5788=ORIENTED_EDGE('',*,*,#4524,.F.);
#5789=ORIENTED_EDGE('',*,*,#4525,.T.);
#5790=ORIENTED_EDGE('',*,*,#4526,.F.);
#5791=ORIENTED_EDGE('',*,*,#4525,.F.);
#5792=ORIENTED_EDGE('',*,*,#4524,.T.);
#5793=ORIENTED_EDGE('',*,*,#4527,.F.);
#5794=ORIENTED_EDGE('',*,*,#4528,.F.);
#5795=ORIENTED_EDGE('',*,*,#4529,.T.);
#5796=ORIENTED_EDGE('',*,*,#4515,.T.);
#5797=ORIENTED_EDGE('',*,*,#4529,.F.);
#5798=ORIENTED_EDGE('',*,*,#4530,.F.);
#5799=ORIENTED_EDGE('',*,*,#4531,.T.);
#5800=ORIENTED_EDGE('',*,*,#4519,.T.);
#5801=ORIENTED_EDGE('',*,*,#4531,.F.);
#5802=ORIENTED_EDGE('',*,*,#4532,.F.);
#5803=ORIENTED_EDGE('',*,*,#4533,.T.);
#5804=ORIENTED_EDGE('',*,*,#4523,.T.);
#5805=ORIENTED_EDGE('',*,*,#4533,.F.);
#5806=ORIENTED_EDGE('',*,*,#4534,.F.);
#5807=ORIENTED_EDGE('',*,*,#4535,.T.);
#5808=ORIENTED_EDGE('',*,*,#4527,.T.);
#5809=ORIENTED_EDGE('',*,*,#4535,.F.);
#5810=ORIENTED_EDGE('',*,*,#4536,.T.);
#5811=ORIENTED_EDGE('',*,*,#4537,.T.);
#5812=ORIENTED_EDGE('',*,*,#4538,.F.);
#5813=ORIENTED_EDGE('',*,*,#4539,.F.);
#5814=ORIENTED_EDGE('',*,*,#4540,.T.);
#5815=ORIENTED_EDGE('',*,*,#4539,.T.);
#5816=ORIENTED_EDGE('',*,*,#4541,.F.);
#5817=ORIENTED_EDGE('',*,*,#4542,.F.);
#5818=ORIENTED_EDGE('',*,*,#4543,.T.);
#5819=ORIENTED_EDGE('',*,*,#4542,.T.);
#5820=ORIENTED_EDGE('',*,*,#4544,.F.);
#5821=ORIENTED_EDGE('',*,*,#4545,.F.);
#5822=ORIENTED_EDGE('',*,*,#4546,.T.);
#5823=ORIENTED_EDGE('',*,*,#4545,.T.);
#5824=ORIENTED_EDGE('',*,*,#4547,.F.);
#5825=ORIENTED_EDGE('',*,*,#4537,.F.);
#5826=ORIENTED_EDGE('',*,*,#4547,.T.);
#5827=ORIENTED_EDGE('',*,*,#4544,.T.);
#5828=ORIENTED_EDGE('',*,*,#4541,.T.);
#5829=ORIENTED_EDGE('',*,*,#4538,.T.);
#5830=ORIENTED_EDGE('',*,*,#4508,.T.);
#5831=ORIENTED_EDGE('',*,*,#4511,.T.);
#5832=ORIENTED_EDGE('',*,*,#4526,.T.);
#5833=ORIENTED_EDGE('',*,*,#4522,.T.);
#5834=ORIENTED_EDGE('',*,*,#4518,.T.);
#5835=ORIENTED_EDGE('',*,*,#4514,.T.);
#5836=ORIENTED_EDGE('',*,*,#4546,.F.);
#5837=ORIENTED_EDGE('',*,*,#4536,.F.);
#5838=ORIENTED_EDGE('',*,*,#4540,.F.);
#5839=ORIENTED_EDGE('',*,*,#4543,.F.);
#5840=ORIENTED_EDGE('',*,*,#4528,.T.);
#5841=ORIENTED_EDGE('',*,*,#4530,.T.);
#5842=ORIENTED_EDGE('',*,*,#4532,.T.);
#5843=ORIENTED_EDGE('',*,*,#4534,.T.);
#5844=ORIENTED_EDGE('',*,*,#4548,.F.);
#5845=ORIENTED_EDGE('',*,*,#4549,.T.);
#5846=ORIENTED_EDGE('',*,*,#4550,.F.);
#5847=ORIENTED_EDGE('',*,*,#4549,.F.);
#5848=ORIENTED_EDGE('',*,*,#4551,.F.);
#5849=ORIENTED_EDGE('',*,*,#4552,.T.);
#5850=ORIENTED_EDGE('',*,*,#4553,.F.);
#5851=ORIENTED_EDGE('',*,*,#4552,.F.);
#5852=ORIENTED_EDGE('',*,*,#4554,.F.);
#5853=ORIENTED_EDGE('',*,*,#4555,.T.);
#5854=ORIENTED_EDGE('',*,*,#4556,.F.);
#5855=ORIENTED_EDGE('',*,*,#4557,.F.);
#5856=ORIENTED_EDGE('',*,*,#4553,.T.);
#5857=ORIENTED_EDGE('',*,*,#4556,.T.);
#5858=ORIENTED_EDGE('',*,*,#4558,.T.);
#5859=ORIENTED_EDGE('',*,*,#4559,.T.);
#5860=ORIENTED_EDGE('',*,*,#4560,.T.);
#5861=ORIENTED_EDGE('',*,*,#4554,.T.);
#5862=ORIENTED_EDGE('',*,*,#4561,.T.);
#5863=ORIENTED_EDGE('',*,*,#4562,.F.);
#5864=ORIENTED_EDGE('',*,*,#4563,.F.);
#5865=ORIENTED_EDGE('',*,*,#4564,.F.);
#5866=ORIENTED_EDGE('',*,*,#4565,.T.);
#5867=ORIENTED_EDGE('',*,*,#4566,.F.);
#5868=ORIENTED_EDGE('',*,*,#4567,.F.);
#5869=ORIENTED_EDGE('',*,*,#4550,.T.);
#5870=ORIENTED_EDGE('',*,*,#4564,.T.);
#5871=ORIENTED_EDGE('',*,*,#4568,.T.);
#5872=ORIENTED_EDGE('',*,*,#4569,.T.);
#5873=ORIENTED_EDGE('',*,*,#4570,.T.);
#5874=ORIENTED_EDGE('',*,*,#4571,.T.);
#5875=ORIENTED_EDGE('',*,*,#4558,.F.);
#5876=ORIENTED_EDGE('',*,*,#4555,.F.);
#5877=ORIENTED_EDGE('',*,*,#4563,.T.);
#5878=ORIENTED_EDGE('',*,*,#4572,.F.);
#5879=ORIENTED_EDGE('',*,*,#4573,.F.);
#5880=ORIENTED_EDGE('',*,*,#4565,.F.);
#5881=ORIENTED_EDGE('',*,*,#4570,.F.);
#5882=ORIENTED_EDGE('',*,*,#4566,.T.);
#5883=ORIENTED_EDGE('',*,*,#4573,.T.);
#5884=ORIENTED_EDGE('',*,*,#4574,.F.);
#5885=ORIENTED_EDGE('',*,*,#4575,.F.);
#5886=ORIENTED_EDGE('',*,*,#4576,.T.);
#5887=ORIENTED_EDGE('',*,*,#4568,.F.);
#5888=ORIENTED_EDGE('',*,*,#4567,.T.);
#5889=ORIENTED_EDGE('',*,*,#4575,.T.);
#5890=ORIENTED_EDGE('',*,*,#4577,.F.);
#5891=ORIENTED_EDGE('',*,*,#4561,.F.);
#5892=ORIENTED_EDGE('',*,*,#4557,.T.);
#5893=ORIENTED_EDGE('',*,*,#4560,.F.);
#5894=ORIENTED_EDGE('',*,*,#4577,.T.);
#5895=ORIENTED_EDGE('',*,*,#4574,.T.);
#5896=ORIENTED_EDGE('',*,*,#4572,.T.);
#5897=ORIENTED_EDGE('',*,*,#4562,.T.);
#5898=ORIENTED_EDGE('',*,*,#4576,.F.);
#5899=ORIENTED_EDGE('',*,*,#4559,.F.);
#5900=ORIENTED_EDGE('',*,*,#4571,.F.);
#5901=ORIENTED_EDGE('',*,*,#4569,.F.);
#5902=ORIENTED_EDGE('',*,*,#4548,.T.);
#5903=ORIENTED_EDGE('',*,*,#4551,.T.);
#5904=ORIENTED_EDGE('',*,*,#4578,.F.);
#5905=ORIENTED_EDGE('',*,*,#4579,.T.);
#5906=ORIENTED_EDGE('',*,*,#4580,.F.);
#5907=ORIENTED_EDGE('',*,*,#4579,.F.);
#5908=ORIENTED_EDGE('',*,*,#4578,.T.);
#5909=ORIENTED_EDGE('',*,*,#4581,.F.);
#5910=ORIENTED_EDGE('',*,*,#4582,.F.);
#5911=ORIENTED_EDGE('',*,*,#4583,.T.);
#5912=ORIENTED_EDGE('',*,*,#4581,.T.);
#5913=ORIENTED_EDGE('',*,*,#4583,.F.);
#5914=ORIENTED_EDGE('',*,*,#4584,.T.);
#5915=ORIENTED_EDGE('',*,*,#4585,.F.);
#5916=ORIENTED_EDGE('',*,*,#4586,.F.);
#5917=ORIENTED_EDGE('',*,*,#4587,.F.);
#5918=ORIENTED_EDGE('',*,*,#4588,.F.);
#5919=ORIENTED_EDGE('',*,*,#4584,.F.);
#5920=ORIENTED_EDGE('',*,*,#4589,.T.);
#5921=ORIENTED_EDGE('',*,*,#4590,.T.);
#5922=ORIENTED_EDGE('',*,*,#4589,.F.);
#5923=ORIENTED_EDGE('',*,*,#4587,.T.);
#5924=ORIENTED_EDGE('',*,*,#4591,.T.);
#5925=ORIENTED_EDGE('',*,*,#4592,.F.);
#5926=ORIENTED_EDGE('',*,*,#4593,.F.);
#5927=ORIENTED_EDGE('',*,*,#4594,.T.);
#5928=ORIENTED_EDGE('',*,*,#4595,.F.);
#5929=ORIENTED_EDGE('',*,*,#4596,.T.);
#5930=ORIENTED_EDGE('',*,*,#4597,.F.);
#5931=ORIENTED_EDGE('',*,*,#4586,.T.);
#5932=ORIENTED_EDGE('',*,*,#4598,.T.);
#5933=ORIENTED_EDGE('',*,*,#4599,.T.);
#5934=ORIENTED_EDGE('',*,*,#4600,.T.);
#5935=ORIENTED_EDGE('',*,*,#4601,.T.);
#5936=ORIENTED_EDGE('',*,*,#4602,.T.);
#5937=ORIENTED_EDGE('',*,*,#4603,.F.);
#5938=ORIENTED_EDGE('',*,*,#4591,.F.);
#5939=ORIENTED_EDGE('',*,*,#4604,.F.);
#5940=ORIENTED_EDGE('',*,*,#4605,.T.);
#5941=ORIENTED_EDGE('',*,*,#4606,.F.);
#5942=ORIENTED_EDGE('',*,*,#4605,.F.);
#5943=ORIENTED_EDGE('',*,*,#4604,.T.);
#5944=ORIENTED_EDGE('',*,*,#4607,.F.);
#5945=ORIENTED_EDGE('',*,*,#4608,.F.);
#5946=ORIENTED_EDGE('',*,*,#4609,.T.);
#5947=ORIENTED_EDGE('',*,*,#4607,.T.);
#5948=ORIENTED_EDGE('',*,*,#4609,.F.);
#5949=ORIENTED_EDGE('',*,*,#4610,.T.);
#5950=ORIENTED_EDGE('',*,*,#4611,.F.);
#5951=ORIENTED_EDGE('',*,*,#4612,.F.);
#5952=ORIENTED_EDGE('',*,*,#4613,.F.);
#5953=ORIENTED_EDGE('',*,*,#4594,.F.);
#5954=ORIENTED_EDGE('',*,*,#4610,.F.);
#5955=ORIENTED_EDGE('',*,*,#4614,.T.);
#5956=ORIENTED_EDGE('',*,*,#4615,.T.);
#5957=ORIENTED_EDGE('',*,*,#4614,.F.);
#5958=ORIENTED_EDGE('',*,*,#4613,.T.);
#5959=ORIENTED_EDGE('',*,*,#4616,.T.);
#5960=ORIENTED_EDGE('',*,*,#4617,.F.);
#5961=ORIENTED_EDGE('',*,*,#4595,.T.);
#5962=ORIENTED_EDGE('',*,*,#4612,.T.);
#5963=ORIENTED_EDGE('',*,*,#4618,.F.);
#5964=ORIENTED_EDGE('',*,*,#4619,.F.);
#5965=ORIENTED_EDGE('',*,*,#4616,.F.);
#5966=ORIENTED_EDGE('',*,*,#4620,.F.);
#5967=ORIENTED_EDGE('',*,*,#4621,.T.);
#5968=ORIENTED_EDGE('',*,*,#4622,.F.);
#5969=ORIENTED_EDGE('',*,*,#4621,.F.);
#5970=ORIENTED_EDGE('',*,*,#4620,.T.);
#5971=ORIENTED_EDGE('',*,*,#4623,.F.);
#5972=ORIENTED_EDGE('',*,*,#4624,.F.);
#5973=ORIENTED_EDGE('',*,*,#4625,.T.);
#5974=ORIENTED_EDGE('',*,*,#4623,.T.);
#5975=ORIENTED_EDGE('',*,*,#4625,.F.);
#5976=ORIENTED_EDGE('',*,*,#4626,.T.);
#5977=ORIENTED_EDGE('',*,*,#4601,.F.);
#5978=ORIENTED_EDGE('',*,*,#4627,.F.);
#5979=ORIENTED_EDGE('',*,*,#4628,.F.);
#5980=ORIENTED_EDGE('',*,*,#4629,.F.);
#5981=ORIENTED_EDGE('',*,*,#4626,.F.);
#5982=ORIENTED_EDGE('',*,*,#4630,.T.);
#5983=ORIENTED_EDGE('',*,*,#4631,.T.);
#5984=ORIENTED_EDGE('',*,*,#4630,.F.);
#5985=ORIENTED_EDGE('',*,*,#4628,.T.);
#5986=ORIENTED_EDGE('',*,*,#4632,.T.);
#5987=ORIENTED_EDGE('',*,*,#4633,.F.);
#5988=ORIENTED_EDGE('',*,*,#4634,.T.);
#5989=ORIENTED_EDGE('',*,*,#4627,.T.);
#5990=ORIENTED_EDGE('',*,*,#4600,.F.);
#5991=ORIENTED_EDGE('',*,*,#4635,.F.);
#5992=ORIENTED_EDGE('',*,*,#4632,.F.);
#5993=ORIENTED_EDGE('',*,*,#4636,.F.);
#5994=ORIENTED_EDGE('',*,*,#4637,.T.);
#5995=ORIENTED_EDGE('',*,*,#4638,.F.);
#5996=ORIENTED_EDGE('',*,*,#4637,.F.);
#5997=ORIENTED_EDGE('',*,*,#4636,.T.);
#5998=ORIENTED_EDGE('',*,*,#4639,.F.);
#5999=ORIENTED_EDGE('',*,*,#4640,.F.);
#6000=ORIENTED_EDGE('',*,*,#4641,.T.);
#6001=ORIENTED_EDGE('',*,*,#4639,.T.);
#6002=ORIENTED_EDGE('',*,*,#4641,.F.);
#6003=ORIENTED_EDGE('',*,*,#4642,.T.);
#6004=ORIENTED_EDGE('',*,*,#4643,.F.);
#6005=ORIENTED_EDGE('',*,*,#4644,.F.);
#6006=ORIENTED_EDGE('',*,*,#4645,.F.);
#6007=ORIENTED_EDGE('',*,*,#4646,.F.);
#6008=ORIENTED_EDGE('',*,*,#4642,.F.);
#6009=ORIENTED_EDGE('',*,*,#4647,.T.);
#6010=ORIENTED_EDGE('',*,*,#4648,.T.);
#6011=ORIENTED_EDGE('',*,*,#4647,.F.);
#6012=ORIENTED_EDGE('',*,*,#4611,.T.);
#6013=ORIENTED_EDGE('',*,*,#4593,.T.);
#6014=ORIENTED_EDGE('',*,*,#4649,.F.);
#6015=ORIENTED_EDGE('',*,*,#4650,.F.);
#6016=ORIENTED_EDGE('',*,*,#4645,.T.);
#6017=ORIENTED_EDGE('',*,*,#4651,.T.);
#6018=ORIENTED_EDGE('',*,*,#4652,.T.);
#6019=ORIENTED_EDGE('',*,*,#4618,.T.);
#6020=ORIENTED_EDGE('',*,*,#4644,.T.);
#6021=ORIENTED_EDGE('',*,*,#4653,.F.);
#6022=ORIENTED_EDGE('',*,*,#4654,.F.);
#6023=ORIENTED_EDGE('',*,*,#4651,.F.);
#6024=ORIENTED_EDGE('',*,*,#4655,.F.);
#6025=ORIENTED_EDGE('',*,*,#4656,.T.);
#6026=ORIENTED_EDGE('',*,*,#4657,.F.);
#6027=ORIENTED_EDGE('',*,*,#4658,.F.);
#6028=ORIENTED_EDGE('',*,*,#4659,.F.);
#6029=ORIENTED_EDGE('',*,*,#4658,.T.);
#6030=ORIENTED_EDGE('',*,*,#4660,.F.);
#6031=ORIENTED_EDGE('',*,*,#4661,.F.);
#6032=ORIENTED_EDGE('',*,*,#4662,.F.);
#6033=ORIENTED_EDGE('',*,*,#4661,.T.);
#6034=ORIENTED_EDGE('',*,*,#4663,.F.);
#6035=ORIENTED_EDGE('',*,*,#4664,.F.);
#6036=ORIENTED_EDGE('',*,*,#4665,.F.);
#6037=ORIENTED_EDGE('',*,*,#4664,.T.);
#6038=ORIENTED_EDGE('',*,*,#4666,.F.);
#6039=ORIENTED_EDGE('',*,*,#4656,.F.);
#6040=ORIENTED_EDGE('',*,*,#4585,.T.);
#6041=ORIENTED_EDGE('',*,*,#4667,.F.);
#6042=ORIENTED_EDGE('',*,*,#4668,.F.);
#6043=ORIENTED_EDGE('',*,*,#4598,.F.);
#6044=ORIENTED_EDGE('',*,*,#4590,.F.);
#6045=ORIENTED_EDGE('',*,*,#4582,.T.);
#6046=ORIENTED_EDGE('',*,*,#4588,.T.);
#6047=ORIENTED_EDGE('',*,*,#4597,.T.);
#6048=ORIENTED_EDGE('',*,*,#4669,.F.);
#6049=ORIENTED_EDGE('',*,*,#4667,.T.);
#6050=ORIENTED_EDGE('',*,*,#4668,.T.);
#6051=ORIENTED_EDGE('',*,*,#4669,.T.);
#6052=ORIENTED_EDGE('',*,*,#4596,.F.);
#6053=ORIENTED_EDGE('',*,*,#4617,.T.);
#6054=ORIENTED_EDGE('',*,*,#4619,.T.);
#6055=ORIENTED_EDGE('',*,*,#4652,.F.);
#6056=ORIENTED_EDGE('',*,*,#4654,.T.);
#6057=ORIENTED_EDGE('',*,*,#4670,.T.);
#6058=ORIENTED_EDGE('',*,*,#4671,.F.);
#6059=ORIENTED_EDGE('',*,*,#4633,.T.);
#6060=ORIENTED_EDGE('',*,*,#4635,.T.);
#6061=ORIENTED_EDGE('',*,*,#4599,.F.);
#6062=ORIENTED_EDGE('',*,*,#4662,.T.);
#6063=ORIENTED_EDGE('',*,*,#4665,.T.);
#6064=ORIENTED_EDGE('',*,*,#4655,.T.);
#6065=ORIENTED_EDGE('',*,*,#4659,.T.);
#6066=ORIENTED_EDGE('',*,*,#4615,.F.);
#6067=ORIENTED_EDGE('',*,*,#4608,.T.);
#6068=ORIENTED_EDGE('',*,*,#4631,.F.);
#6069=ORIENTED_EDGE('',*,*,#4624,.T.);
#6070=ORIENTED_EDGE('',*,*,#4643,.T.);
#6071=ORIENTED_EDGE('',*,*,#4672,.T.);
#6072=ORIENTED_EDGE('',*,*,#4670,.F.);
#6073=ORIENTED_EDGE('',*,*,#4653,.T.);
#6074=ORIENTED_EDGE('',*,*,#4648,.F.);
#6075=ORIENTED_EDGE('',*,*,#4640,.T.);
#6076=ORIENTED_EDGE('',*,*,#4629,.T.);
#6077=ORIENTED_EDGE('',*,*,#4634,.F.);
#6078=ORIENTED_EDGE('',*,*,#4671,.T.);
#6079=ORIENTED_EDGE('',*,*,#4672,.F.);
#6080=ORIENTED_EDGE('',*,*,#4646,.T.);
#6081=ORIENTED_EDGE('',*,*,#4650,.T.);
#6082=ORIENTED_EDGE('',*,*,#4673,.F.);
#6083=ORIENTED_EDGE('',*,*,#4602,.F.);
#6084=ORIENTED_EDGE('',*,*,#4673,.T.);
#6085=ORIENTED_EDGE('',*,*,#4649,.T.);
#6086=ORIENTED_EDGE('',*,*,#4592,.T.);
#6087=ORIENTED_EDGE('',*,*,#4603,.T.);
#6088=ORIENTED_EDGE('',*,*,#4580,.T.);
#6089=ORIENTED_EDGE('',*,*,#4606,.T.);
#6090=ORIENTED_EDGE('',*,*,#4622,.T.);
#6091=ORIENTED_EDGE('',*,*,#4638,.T.);
#6092=ORIENTED_EDGE('',*,*,#4663,.T.);
#6093=ORIENTED_EDGE('',*,*,#4660,.T.);
#6094=ORIENTED_EDGE('',*,*,#4657,.T.);
#6095=ORIENTED_EDGE('',*,*,#4666,.T.);
#6096=ORIENTED_EDGE('',*,*,#4674,.T.);
#6097=ORIENTED_EDGE('',*,*,#4675,.T.);
#6098=ORIENTED_EDGE('',*,*,#4676,.F.);
#6099=ORIENTED_EDGE('',*,*,#4677,.F.);
#6100=ORIENTED_EDGE('',*,*,#4678,.T.);
#6101=ORIENTED_EDGE('',*,*,#4677,.T.);
#6102=ORIENTED_EDGE('',*,*,#4679,.F.);
#6103=ORIENTED_EDGE('',*,*,#4680,.F.);
#6104=ORIENTED_EDGE('',*,*,#4681,.T.);
#6105=ORIENTED_EDGE('',*,*,#4680,.T.);
#6106=ORIENTED_EDGE('',*,*,#4682,.F.);
#6107=ORIENTED_EDGE('',*,*,#4683,.F.);
#6108=ORIENTED_EDGE('',*,*,#4684,.T.);
#6109=ORIENTED_EDGE('',*,*,#4683,.T.);
#6110=ORIENTED_EDGE('',*,*,#4685,.F.);
#6111=ORIENTED_EDGE('',*,*,#4675,.F.);
#6112=ORIENTED_EDGE('',*,*,#4685,.T.);
#6113=ORIENTED_EDGE('',*,*,#4682,.T.);
#6114=ORIENTED_EDGE('',*,*,#4679,.T.);
#6115=ORIENTED_EDGE('',*,*,#4676,.T.);
#6116=ORIENTED_EDGE('',*,*,#4684,.F.);
#6117=ORIENTED_EDGE('',*,*,#4674,.F.);
#6118=ORIENTED_EDGE('',*,*,#4678,.F.);
#6119=ORIENTED_EDGE('',*,*,#4681,.F.);
#6120=ORIENTED_EDGE('',*,*,#4686,.T.);
#6121=ORIENTED_EDGE('',*,*,#4687,.T.);
#6122=ORIENTED_EDGE('',*,*,#4688,.F.);
#6123=ORIENTED_EDGE('',*,*,#4689,.F.);
#6124=ORIENTED_EDGE('',*,*,#4690,.T.);
#6125=ORIENTED_EDGE('',*,*,#4689,.T.);
#6126=ORIENTED_EDGE('',*,*,#4691,.F.);
#6127=ORIENTED_EDGE('',*,*,#4692,.F.);
#6128=ORIENTED_EDGE('',*,*,#4693,.T.);
#6129=ORIENTED_EDGE('',*,*,#4692,.T.);
#6130=ORIENTED_EDGE('',*,*,#4694,.F.);
#6131=ORIENTED_EDGE('',*,*,#4695,.F.);
#6132=ORIENTED_EDGE('',*,*,#4696,.T.);
#6133=ORIENTED_EDGE('',*,*,#4695,.T.);
#6134=ORIENTED_EDGE('',*,*,#4697,.F.);
#6135=ORIENTED_EDGE('',*,*,#4687,.F.);
#6136=ORIENTED_EDGE('',*,*,#4697,.T.);
#6137=ORIENTED_EDGE('',*,*,#4694,.T.);
#6138=ORIENTED_EDGE('',*,*,#4691,.T.);
#6139=ORIENTED_EDGE('',*,*,#4688,.T.);
#6140=ORIENTED_EDGE('',*,*,#4696,.F.);
#6141=ORIENTED_EDGE('',*,*,#4686,.F.);
#6142=ORIENTED_EDGE('',*,*,#4690,.F.);
#6143=ORIENTED_EDGE('',*,*,#4693,.F.);
#6144=ORIENTED_EDGE('',*,*,#4698,.T.);
#6145=ORIENTED_EDGE('',*,*,#4699,.T.);
#6146=ORIENTED_EDGE('',*,*,#4700,.T.);
#6147=ORIENTED_EDGE('',*,*,#4701,.F.);
#6148=ORIENTED_EDGE('',*,*,#4702,.T.);
#6149=ORIENTED_EDGE('',*,*,#4703,.T.);
#6150=ORIENTED_EDGE('',*,*,#4704,.T.);
#6151=ORIENTED_EDGE('',*,*,#4699,.F.);
#6152=ORIENTED_EDGE('',*,*,#4705,.T.);
#6153=ORIENTED_EDGE('',*,*,#4706,.T.);
#6154=ORIENTED_EDGE('',*,*,#4707,.T.);
#6155=ORIENTED_EDGE('',*,*,#4703,.F.);
#6156=ORIENTED_EDGE('',*,*,#4708,.T.);
#6157=ORIENTED_EDGE('',*,*,#4709,.T.);
#6158=ORIENTED_EDGE('',*,*,#4710,.T.);
#6159=ORIENTED_EDGE('',*,*,#4706,.F.);
#6160=ORIENTED_EDGE('',*,*,#4711,.T.);
#6161=ORIENTED_EDGE('',*,*,#4712,.T.);
#6162=ORIENTED_EDGE('',*,*,#4713,.T.);
#6163=ORIENTED_EDGE('',*,*,#4709,.F.);
#6164=ORIENTED_EDGE('',*,*,#4714,.T.);
#6165=ORIENTED_EDGE('',*,*,#4701,.T.);
#6166=ORIENTED_EDGE('',*,*,#4715,.T.);
#6167=ORIENTED_EDGE('',*,*,#4712,.F.);
#6168=ORIENTED_EDGE('',*,*,#4714,.F.);
#6169=ORIENTED_EDGE('',*,*,#4711,.F.);
#6170=ORIENTED_EDGE('',*,*,#4708,.F.);
#6171=ORIENTED_EDGE('',*,*,#4705,.F.);
#6172=ORIENTED_EDGE('',*,*,#4702,.F.);
#6173=ORIENTED_EDGE('',*,*,#4698,.F.);
#6174=ORIENTED_EDGE('',*,*,#4715,.F.);
#6175=ORIENTED_EDGE('',*,*,#4700,.F.);
#6176=ORIENTED_EDGE('',*,*,#4704,.F.);
#6177=ORIENTED_EDGE('',*,*,#4707,.F.);
#6178=ORIENTED_EDGE('',*,*,#4710,.F.);
#6179=ORIENTED_EDGE('',*,*,#4713,.F.);
#6180=ORIENTED_EDGE('',*,*,#4716,.F.);
#6181=ORIENTED_EDGE('',*,*,#4717,.F.);
#6182=ORIENTED_EDGE('',*,*,#4718,.F.);
#6183=ORIENTED_EDGE('',*,*,#4719,.T.);
#6184=ORIENTED_EDGE('',*,*,#4717,.T.);
#6185=ORIENTED_EDGE('',*,*,#4719,.F.);
#6186=ORIENTED_EDGE('',*,*,#4720,.F.);
#6187=ORIENTED_EDGE('',*,*,#4721,.T.);
#6188=ORIENTED_EDGE('',*,*,#4718,.T.);
#6189=ORIENTED_EDGE('',*,*,#4721,.F.);
#6190=ORIENTED_EDGE('',*,*,#4722,.F.);
#6191=ORIENTED_EDGE('',*,*,#4723,.T.);
#6192=ORIENTED_EDGE('',*,*,#4720,.T.);
#6193=ORIENTED_EDGE('',*,*,#4723,.F.);
#6194=ORIENTED_EDGE('',*,*,#4722,.T.);
#6195=ORIENTED_EDGE('',*,*,#4724,.F.);
#6196=ORIENTED_EDGE('',*,*,#4725,.F.);
#6197=ORIENTED_EDGE('',*,*,#4726,.T.);
#6198=ORIENTED_EDGE('',*,*,#4724,.T.);
#6199=ORIENTED_EDGE('',*,*,#4726,.F.);
#6200=ORIENTED_EDGE('',*,*,#4716,.T.);
#6201=ORIENTED_EDGE('',*,*,#4727,.T.);
#6202=ORIENTED_EDGE('',*,*,#4725,.T.);
#6203=ORIENTED_EDGE('',*,*,#4727,.F.);
#6204=ORIENTED_EDGE('',*,*,#4728,.F.);
#6205=ORIENTED_EDGE('',*,*,#4729,.F.);
#6206=ORIENTED_EDGE('',*,*,#4730,.T.);
#6207=ORIENTED_EDGE('',*,*,#4731,.F.);
#6208=ORIENTED_EDGE('',*,*,#4732,.F.);
#6209=ORIENTED_EDGE('',*,*,#4730,.F.);
#6210=ORIENTED_EDGE('',*,*,#4731,.T.);
#6211=ORIENTED_EDGE('',*,*,#4732,.T.);
#6212=ORIENTED_EDGE('',*,*,#4733,.T.);
#6213=ORIENTED_EDGE('',*,*,#4734,.T.);
#6214=ORIENTED_EDGE('',*,*,#4733,.F.);
#6215=ORIENTED_EDGE('',*,*,#4735,.T.);
#6216=ORIENTED_EDGE('',*,*,#4736,.T.);
#6217=ORIENTED_EDGE('',*,*,#4737,.F.);
#6218=ORIENTED_EDGE('',*,*,#4736,.F.);
#6219=ORIENTED_EDGE('',*,*,#4737,.T.);
#6220=ORIENTED_EDGE('',*,*,#4738,.T.);
#6221=ORIENTED_EDGE('',*,*,#4739,.F.);
#6222=ORIENTED_EDGE('',*,*,#4738,.F.);
#6223=ORIENTED_EDGE('',*,*,#4734,.F.);
#6224=ORIENTED_EDGE('',*,*,#4739,.T.);
#6225=ORIENTED_EDGE('',*,*,#4740,.F.);
#6226=ORIENTED_EDGE('',*,*,#4741,.T.);
#6227=ORIENTED_EDGE('',*,*,#4728,.T.);
#6228=ORIENTED_EDGE('',*,*,#4729,.T.);
#6229=ORIENTED_EDGE('',*,*,#4741,.F.);
#6230=ORIENTED_EDGE('',*,*,#4740,.T.);
#6231=ORIENTED_EDGE('',*,*,#4742,.F.);
#6232=ORIENTED_EDGE('',*,*,#4742,.T.);
#6233=ORIENTED_EDGE('',*,*,#4743,.T.);
#6234=ORIENTED_EDGE('',*,*,#4735,.F.);
#6235=ORIENTED_EDGE('',*,*,#4743,.F.);
#6236=ORIENTED_EDGE('',*,*,#4744,.F.);
#6237=ORIENTED_EDGE('',*,*,#4745,.F.);
#6238=ORIENTED_EDGE('',*,*,#4746,.T.);
#6239=ORIENTED_EDGE('',*,*,#4747,.F.);
#6240=ORIENTED_EDGE('',*,*,#4748,.F.);
#6241=ORIENTED_EDGE('',*,*,#4746,.F.);
#6242=ORIENTED_EDGE('',*,*,#4749,.T.);
#6243=ORIENTED_EDGE('',*,*,#4750,.T.);
#6244=ORIENTED_EDGE('',*,*,#4747,.T.);
#6245=ORIENTED_EDGE('',*,*,#4748,.T.);
#6246=ORIENTED_EDGE('',*,*,#4750,.F.);
#6247=ORIENTED_EDGE('',*,*,#4751,.F.);
#6248=ORIENTED_EDGE('',*,*,#4752,.T.);
#6249=ORIENTED_EDGE('',*,*,#4753,.F.);
#6250=ORIENTED_EDGE('',*,*,#4754,.T.);
#6251=ORIENTED_EDGE('',*,*,#4751,.T.);
#6252=ORIENTED_EDGE('',*,*,#4754,.F.);
#6253=ORIENTED_EDGE('',*,*,#4755,.F.);
#6254=ORIENTED_EDGE('',*,*,#4756,.T.);
#6255=ORIENTED_EDGE('',*,*,#4753,.T.);
#6256=ORIENTED_EDGE('',*,*,#4756,.F.);
#6257=ORIENTED_EDGE('',*,*,#4757,.F.);
#6258=ORIENTED_EDGE('',*,*,#4758,.T.);
#6259=ORIENTED_EDGE('',*,*,#4755,.T.);
#6260=ORIENTED_EDGE('',*,*,#4758,.F.);
#6261=ORIENTED_EDGE('',*,*,#4757,.T.);
#6262=ORIENTED_EDGE('',*,*,#4749,.F.);
#6263=ORIENTED_EDGE('',*,*,#4744,.T.);
#6264=ORIENTED_EDGE('',*,*,#4745,.T.);
#6265=ORIENTED_EDGE('',*,*,#4759,.T.);
#6266=ORIENTED_EDGE('',*,*,#4752,.F.);
#6267=ORIENTED_EDGE('',*,*,#4759,.F.);
#6268=ORIENTED_EDGE('',*,*,#4760,.T.);
#6269=ORIENTED_EDGE('',*,*,#4760,.F.);
#6270=ORIENTED_EDGE('',*,*,#4761,.T.);
#6271=ORIENTED_EDGE('',*,*,#4761,.F.);
#6272=ORIENTED_EDGE('',*,*,#4762,.T.);
#6273=ORIENTED_EDGE('',*,*,#4762,.F.);
#6274=ORIENTED_EDGE('',*,*,#4763,.T.);
#6275=ORIENTED_EDGE('',*,*,#4763,.F.);
#6276=ORIENTED_EDGE('',*,*,#4764,.T.);
#6277=ORIENTED_EDGE('',*,*,#4764,.F.);
#6278=ORIENTED_EDGE('',*,*,#4765,.T.);
#6279=ORIENTED_EDGE('',*,*,#4765,.F.);
#6280=ORIENTED_EDGE('',*,*,#4766,.T.);
#6281=ORIENTED_EDGE('',*,*,#4766,.F.);
#6282=ORIENTED_EDGE('',*,*,#4767,.F.);
#6283=ORIENTED_EDGE('',*,*,#4768,.F.);
#6284=ORIENTED_EDGE('',*,*,#4769,.F.);
#6285=ORIENTED_EDGE('',*,*,#4770,.F.);
#6286=ORIENTED_EDGE('',*,*,#4769,.T.);
#6287=ORIENTED_EDGE('',*,*,#4771,.F.);
#6288=ORIENTED_EDGE('',*,*,#4772,.T.);
#6289=ORIENTED_EDGE('',*,*,#4773,.F.);
#6290=ORIENTED_EDGE('',*,*,#4774,.T.);
#6291=ORIENTED_EDGE('',*,*,#4775,.F.);
#6292=ORIENTED_EDGE('',*,*,#4776,.T.);
#6293=ORIENTED_EDGE('',*,*,#4777,.F.);
#6294=ORIENTED_EDGE('',*,*,#4776,.F.);
#6295=ORIENTED_EDGE('',*,*,#4778,.F.);
#6296=ORIENTED_EDGE('',*,*,#4779,.T.);
#6297=ORIENTED_EDGE('',*,*,#4780,.F.);
#6298=ORIENTED_EDGE('',*,*,#4781,.T.);
#6299=ORIENTED_EDGE('',*,*,#4782,.F.);
#6300=ORIENTED_EDGE('',*,*,#4783,.T.);
#6301=ORIENTED_EDGE('',*,*,#4784,.F.);
#6302=ORIENTED_EDGE('',*,*,#4785,.T.);
#6303=ORIENTED_EDGE('',*,*,#4786,.F.);
#6304=ORIENTED_EDGE('',*,*,#4768,.T.);
#6305=ORIENTED_EDGE('',*,*,#4787,.T.);
#6306=ORIENTED_EDGE('',*,*,#4788,.T.);
#6307=ORIENTED_EDGE('',*,*,#4771,.T.);
#6308=ORIENTED_EDGE('',*,*,#4789,.F.);
#6309=ORIENTED_EDGE('',*,*,#4790,.F.);
#6310=ORIENTED_EDGE('',*,*,#4772,.F.);
#6311=ORIENTED_EDGE('',*,*,#4788,.F.);
#6312=ORIENTED_EDGE('',*,*,#4790,.T.);
#6313=ORIENTED_EDGE('',*,*,#4791,.T.);
#6314=ORIENTED_EDGE('',*,*,#4792,.T.);
#6315=ORIENTED_EDGE('',*,*,#4773,.T.);
#6316=ORIENTED_EDGE('',*,*,#4793,.F.);
#6317=ORIENTED_EDGE('',*,*,#4794,.F.);
#6318=ORIENTED_EDGE('',*,*,#4774,.F.);
#6319=ORIENTED_EDGE('',*,*,#4792,.F.);
#6320=ORIENTED_EDGE('',*,*,#4794,.T.);
#6321=ORIENTED_EDGE('',*,*,#4795,.T.);
#6322=ORIENTED_EDGE('',*,*,#4796,.T.);
#6323=ORIENTED_EDGE('',*,*,#4797,.T.);
#6324=ORIENTED_EDGE('',*,*,#4778,.T.);
#6325=ORIENTED_EDGE('',*,*,#4775,.T.);
#6326=ORIENTED_EDGE('',*,*,#4798,.F.);
#6327=ORIENTED_EDGE('',*,*,#4799,.F.);
#6328=ORIENTED_EDGE('',*,*,#4779,.F.);
#6329=ORIENTED_EDGE('',*,*,#4797,.F.);
#6330=ORIENTED_EDGE('',*,*,#4799,.T.);
#6331=ORIENTED_EDGE('',*,*,#4800,.T.);
#6332=ORIENTED_EDGE('',*,*,#4801,.T.);
#6333=ORIENTED_EDGE('',*,*,#4780,.T.);
#6334=ORIENTED_EDGE('',*,*,#4802,.F.);
#6335=ORIENTED_EDGE('',*,*,#4803,.F.);
#6336=ORIENTED_EDGE('',*,*,#4781,.F.);
#6337=ORIENTED_EDGE('',*,*,#4801,.F.);
#6338=ORIENTED_EDGE('',*,*,#4803,.T.);
#6339=ORIENTED_EDGE('',*,*,#4804,.T.);
#6340=ORIENTED_EDGE('',*,*,#4805,.T.);
#6341=ORIENTED_EDGE('',*,*,#4782,.T.);
#6342=ORIENTED_EDGE('',*,*,#4783,.F.);
#6343=ORIENTED_EDGE('',*,*,#4805,.F.);
#6344=ORIENTED_EDGE('',*,*,#4806,.F.);
#6345=ORIENTED_EDGE('',*,*,#4807,.F.);
#6346=ORIENTED_EDGE('',*,*,#4808,.F.);
#6347=ORIENTED_EDGE('',*,*,#4809,.T.);
#6348=ORIENTED_EDGE('',*,*,#4795,.F.);
#6349=ORIENTED_EDGE('',*,*,#4793,.T.);
#6350=ORIENTED_EDGE('',*,*,#4791,.F.);
#6351=ORIENTED_EDGE('',*,*,#4789,.T.);
#6352=ORIENTED_EDGE('',*,*,#4787,.F.);
#6353=ORIENTED_EDGE('',*,*,#4767,.T.);
#6354=ORIENTED_EDGE('',*,*,#4810,.F.);
#6355=ORIENTED_EDGE('',*,*,#4811,.T.);
#6356=ORIENTED_EDGE('',*,*,#4812,.F.);
#6357=ORIENTED_EDGE('',*,*,#4806,.T.);
#6358=ORIENTED_EDGE('',*,*,#4804,.F.);
#6359=ORIENTED_EDGE('',*,*,#4802,.T.);
#6360=ORIENTED_EDGE('',*,*,#4800,.F.);
#6361=ORIENTED_EDGE('',*,*,#4798,.T.);
#6362=ORIENTED_EDGE('',*,*,#4796,.F.);
#6363=ORIENTED_EDGE('',*,*,#4809,.F.);
#6364=ORIENTED_EDGE('',*,*,#4770,.T.);
#6365=ORIENTED_EDGE('',*,*,#4786,.T.);
#6366=ORIENTED_EDGE('',*,*,#4813,.T.);
#6367=ORIENTED_EDGE('',*,*,#4810,.T.);
#6368=ORIENTED_EDGE('',*,*,#4785,.F.);
#6369=ORIENTED_EDGE('',*,*,#4814,.F.);
#6370=ORIENTED_EDGE('',*,*,#4811,.F.);
#6371=ORIENTED_EDGE('',*,*,#4813,.F.);
#6372=ORIENTED_EDGE('',*,*,#4777,.T.);
#6373=ORIENTED_EDGE('',*,*,#4808,.T.);
#6374=ORIENTED_EDGE('',*,*,#4807,.T.);
#6375=ORIENTED_EDGE('',*,*,#4812,.T.);
#6376=ORIENTED_EDGE('',*,*,#4814,.T.);
#6377=ORIENTED_EDGE('',*,*,#4784,.T.);
#6378=ORIENTED_EDGE('',*,*,#4815,.F.);
#6379=ORIENTED_EDGE('',*,*,#4816,.T.);
#6380=ORIENTED_EDGE('',*,*,#4817,.F.);
#6381=ORIENTED_EDGE('',*,*,#4818,.T.);
#6382=ORIENTED_EDGE('',*,*,#4815,.T.);
#6383=ORIENTED_EDGE('',*,*,#4818,.F.);
#6384=ORIENTED_EDGE('',*,*,#4817,.T.);
#6385=ORIENTED_EDGE('',*,*,#4819,.F.);
#6386=ORIENTED_EDGE('',*,*,#4819,.T.);
#6387=ORIENTED_EDGE('',*,*,#4820,.T.);
#6388=ORIENTED_EDGE('',*,*,#4816,.F.);
#6389=ORIENTED_EDGE('',*,*,#4820,.F.);
#6390=ORIENTED_EDGE('',*,*,#4821,.F.);
#6391=ORIENTED_EDGE('',*,*,#4822,.T.);
#6392=ORIENTED_EDGE('',*,*,#4823,.F.);
#6393=ORIENTED_EDGE('',*,*,#4824,.T.);
#6394=ORIENTED_EDGE('',*,*,#4821,.T.);
#6395=ORIENTED_EDGE('',*,*,#4824,.F.);
#6396=ORIENTED_EDGE('',*,*,#4823,.T.);
#6397=ORIENTED_EDGE('',*,*,#4825,.F.);
#6398=ORIENTED_EDGE('',*,*,#4825,.T.);
#6399=ORIENTED_EDGE('',*,*,#4826,.T.);
#6400=ORIENTED_EDGE('',*,*,#4822,.F.);
#6401=ORIENTED_EDGE('',*,*,#4826,.F.);
#6402=ORIENTED_EDGE('',*,*,#4827,.F.);
#6403=ORIENTED_EDGE('',*,*,#4828,.F.);
#6404=ORIENTED_EDGE('',*,*,#4829,.T.);
#6405=ORIENTED_EDGE('',*,*,#4830,.F.);
#6406=ORIENTED_EDGE('',*,*,#4831,.F.);
#6407=ORIENTED_EDGE('',*,*,#4829,.F.);
#6408=ORIENTED_EDGE('',*,*,#4830,.T.);
#6409=ORIENTED_EDGE('',*,*,#4831,.T.);
#6410=ORIENTED_EDGE('',*,*,#4832,.T.);
#6411=ORIENTED_EDGE('',*,*,#4833,.T.);
#6412=ORIENTED_EDGE('',*,*,#4832,.F.);
#6413=ORIENTED_EDGE('',*,*,#4834,.T.);
#6414=ORIENTED_EDGE('',*,*,#4835,.T.);
#6415=ORIENTED_EDGE('',*,*,#4836,.F.);
#6416=ORIENTED_EDGE('',*,*,#4835,.F.);
#6417=ORIENTED_EDGE('',*,*,#4836,.T.);
#6418=ORIENTED_EDGE('',*,*,#4837,.T.);
#6419=ORIENTED_EDGE('',*,*,#4838,.F.);
#6420=ORIENTED_EDGE('',*,*,#4837,.F.);
#6421=ORIENTED_EDGE('',*,*,#4833,.F.);
#6422=ORIENTED_EDGE('',*,*,#4838,.T.);
#6423=ORIENTED_EDGE('',*,*,#4839,.F.);
#6424=ORIENTED_EDGE('',*,*,#4840,.T.);
#6425=ORIENTED_EDGE('',*,*,#4827,.T.);
#6426=ORIENTED_EDGE('',*,*,#4828,.T.);
#6427=ORIENTED_EDGE('',*,*,#4840,.F.);
#6428=ORIENTED_EDGE('',*,*,#4839,.T.);
#6429=ORIENTED_EDGE('',*,*,#4841,.F.);
#6430=ORIENTED_EDGE('',*,*,#4841,.T.);
#6431=ORIENTED_EDGE('',*,*,#4842,.T.);
#6432=ORIENTED_EDGE('',*,*,#4834,.F.);
#6433=ORIENTED_EDGE('',*,*,#4842,.F.);
#6434=ORIENTED_EDGE('',*,*,#4843,.F.);
#6435=ORIENTED_EDGE('',*,*,#4844,.F.);
#6436=ORIENTED_EDGE('',*,*,#4845,.T.);
#6437=ORIENTED_EDGE('',*,*,#4846,.F.);
#6438=ORIENTED_EDGE('',*,*,#4847,.F.);
#6439=ORIENTED_EDGE('',*,*,#4845,.F.);
#6440=ORIENTED_EDGE('',*,*,#4848,.T.);
#6441=ORIENTED_EDGE('',*,*,#4849,.T.);
#6442=ORIENTED_EDGE('',*,*,#4846,.T.);
#6443=ORIENTED_EDGE('',*,*,#4847,.T.);
#6444=ORIENTED_EDGE('',*,*,#4849,.F.);
#6445=ORIENTED_EDGE('',*,*,#4850,.F.);
#6446=ORIENTED_EDGE('',*,*,#4851,.T.);
#6447=ORIENTED_EDGE('',*,*,#4852,.F.);
#6448=ORIENTED_EDGE('',*,*,#4853,.T.);
#6449=ORIENTED_EDGE('',*,*,#4850,.T.);
#6450=ORIENTED_EDGE('',*,*,#4853,.F.);
#6451=ORIENTED_EDGE('',*,*,#4854,.F.);
#6452=ORIENTED_EDGE('',*,*,#4855,.T.);
#6453=ORIENTED_EDGE('',*,*,#4852,.T.);
#6454=ORIENTED_EDGE('',*,*,#4855,.F.);
#6455=ORIENTED_EDGE('',*,*,#4856,.F.);
#6456=ORIENTED_EDGE('',*,*,#4857,.T.);
#6457=ORIENTED_EDGE('',*,*,#4854,.T.);
#6458=ORIENTED_EDGE('',*,*,#4857,.F.);
#6459=ORIENTED_EDGE('',*,*,#4856,.T.);
#6460=ORIENTED_EDGE('',*,*,#4848,.F.);
#6461=ORIENTED_EDGE('',*,*,#4843,.T.);
#6462=ORIENTED_EDGE('',*,*,#4844,.T.);
#6463=ORIENTED_EDGE('',*,*,#4858,.T.);
#6464=ORIENTED_EDGE('',*,*,#4851,.F.);
#6465=ORIENTED_EDGE('',*,*,#4858,.F.);
#6466=ORIENTED_EDGE('',*,*,#4859,.T.);
#6467=ORIENTED_EDGE('',*,*,#4859,.F.);
#6468=ORIENTED_EDGE('',*,*,#4860,.T.);
#6469=ORIENTED_EDGE('',*,*,#4860,.F.);
#6470=ORIENTED_EDGE('',*,*,#4861,.T.);
#6471=ORIENTED_EDGE('',*,*,#4861,.F.);
#6472=ORIENTED_EDGE('',*,*,#4862,.T.);
#6473=ORIENTED_EDGE('',*,*,#4862,.F.);
#6474=ORIENTED_EDGE('',*,*,#4863,.T.);
#6475=ORIENTED_EDGE('',*,*,#4863,.F.);
#6476=ORIENTED_EDGE('',*,*,#4864,.T.);
#6477=ORIENTED_EDGE('',*,*,#4864,.F.);
#6478=ORIENTED_EDGE('',*,*,#4865,.T.);
#6479=ORIENTED_EDGE('',*,*,#4865,.F.);
#6480=ORIENTED_EDGE('',*,*,#4866,.T.);
#6481=ORIENTED_EDGE('',*,*,#4866,.F.);
#6482=ORIENTED_EDGE('',*,*,#4867,.F.);
#6483=ORIENTED_EDGE('',*,*,#4868,.F.);
#6484=ORIENTED_EDGE('',*,*,#4869,.F.);
#6485=ORIENTED_EDGE('',*,*,#4870,.F.);
#6486=ORIENTED_EDGE('',*,*,#4869,.T.);
#6487=ORIENTED_EDGE('',*,*,#4871,.F.);
#6488=ORIENTED_EDGE('',*,*,#4872,.T.);
#6489=ORIENTED_EDGE('',*,*,#4873,.F.);
#6490=ORIENTED_EDGE('',*,*,#4874,.T.);
#6491=ORIENTED_EDGE('',*,*,#4875,.F.);
#6492=ORIENTED_EDGE('',*,*,#4876,.T.);
#6493=ORIENTED_EDGE('',*,*,#4877,.T.);
#6494=ORIENTED_EDGE('',*,*,#4878,.F.);
#6495=ORIENTED_EDGE('',*,*,#4877,.F.);
#6496=ORIENTED_EDGE('',*,*,#4879,.T.);
#6497=ORIENTED_EDGE('',*,*,#4880,.F.);
#6498=ORIENTED_EDGE('',*,*,#4881,.T.);
#6499=ORIENTED_EDGE('',*,*,#4882,.F.);
#6500=ORIENTED_EDGE('',*,*,#4883,.T.);
#6501=ORIENTED_EDGE('',*,*,#4884,.F.);
#6502=ORIENTED_EDGE('',*,*,#4885,.T.);
#6503=ORIENTED_EDGE('',*,*,#4886,.F.);
#6504=ORIENTED_EDGE('',*,*,#4887,.T.);
#6505=ORIENTED_EDGE('',*,*,#4888,.F.);
#6506=ORIENTED_EDGE('',*,*,#4868,.T.);
#6507=ORIENTED_EDGE('',*,*,#4889,.T.);
#6508=ORIENTED_EDGE('',*,*,#4890,.T.);
#6509=ORIENTED_EDGE('',*,*,#4871,.T.);
#6510=ORIENTED_EDGE('',*,*,#4891,.F.);
#6511=ORIENTED_EDGE('',*,*,#4892,.F.);
#6512=ORIENTED_EDGE('',*,*,#4872,.F.);
#6513=ORIENTED_EDGE('',*,*,#4890,.F.);
#6514=ORIENTED_EDGE('',*,*,#4892,.T.);
#6515=ORIENTED_EDGE('',*,*,#4893,.T.);
#6516=ORIENTED_EDGE('',*,*,#4894,.T.);
#6517=ORIENTED_EDGE('',*,*,#4873,.T.);
#6518=ORIENTED_EDGE('',*,*,#4895,.F.);
#6519=ORIENTED_EDGE('',*,*,#4896,.F.);
#6520=ORIENTED_EDGE('',*,*,#4874,.F.);
#6521=ORIENTED_EDGE('',*,*,#4894,.F.);
#6522=ORIENTED_EDGE('',*,*,#4896,.T.);
#6523=ORIENTED_EDGE('',*,*,#4897,.T.);
#6524=ORIENTED_EDGE('',*,*,#4898,.T.);
#6525=ORIENTED_EDGE('',*,*,#4875,.T.);
#6526=ORIENTED_EDGE('',*,*,#4899,.F.);
#6527=ORIENTED_EDGE('',*,*,#4900,.F.);
#6528=ORIENTED_EDGE('',*,*,#4879,.F.);
#6529=ORIENTED_EDGE('',*,*,#4876,.F.);
#6530=ORIENTED_EDGE('',*,*,#4898,.F.);
#6531=ORIENTED_EDGE('',*,*,#4901,.F.);
#6532=ORIENTED_EDGE('',*,*,#4900,.T.);
#6533=ORIENTED_EDGE('',*,*,#4902,.T.);
#6534=ORIENTED_EDGE('',*,*,#4903,.T.);
#6535=ORIENTED_EDGE('',*,*,#4880,.T.);
#6536=ORIENTED_EDGE('',*,*,#4904,.F.);
#6537=ORIENTED_EDGE('',*,*,#4905,.F.);
#6538=ORIENTED_EDGE('',*,*,#4881,.F.);
#6539=ORIENTED_EDGE('',*,*,#4903,.F.);
#6540=ORIENTED_EDGE('',*,*,#4905,.T.);
#6541=ORIENTED_EDGE('',*,*,#4906,.T.);
#6542=ORIENTED_EDGE('',*,*,#4907,.T.);
#6543=ORIENTED_EDGE('',*,*,#4882,.T.);
#6544=ORIENTED_EDGE('',*,*,#4908,.F.);
#6545=ORIENTED_EDGE('',*,*,#4909,.F.);
#6546=ORIENTED_EDGE('',*,*,#4883,.F.);
#6547=ORIENTED_EDGE('',*,*,#4907,.F.);
#6548=ORIENTED_EDGE('',*,*,#4909,.T.);
#6549=ORIENTED_EDGE('',*,*,#4910,.T.);
#6550=ORIENTED_EDGE('',*,*,#4911,.T.);
#6551=ORIENTED_EDGE('',*,*,#4884,.T.);
#6552=ORIENTED_EDGE('',*,*,#4885,.F.);
#6553=ORIENTED_EDGE('',*,*,#4911,.F.);
#6554=ORIENTED_EDGE('',*,*,#4912,.F.);
#6555=ORIENTED_EDGE('',*,*,#4913,.F.);
#6556=ORIENTED_EDGE('',*,*,#4914,.F.);
#6557=ORIENTED_EDGE('',*,*,#4915,.T.);
#6558=ORIENTED_EDGE('',*,*,#4901,.T.);
#6559=ORIENTED_EDGE('',*,*,#4897,.F.);
#6560=ORIENTED_EDGE('',*,*,#4895,.T.);
#6561=ORIENTED_EDGE('',*,*,#4893,.F.);
#6562=ORIENTED_EDGE('',*,*,#4891,.T.);
#6563=ORIENTED_EDGE('',*,*,#4889,.F.);
#6564=ORIENTED_EDGE('',*,*,#4867,.T.);
#6565=ORIENTED_EDGE('',*,*,#4916,.F.);
#6566=ORIENTED_EDGE('',*,*,#4917,.T.);
#6567=ORIENTED_EDGE('',*,*,#4918,.F.);
#6568=ORIENTED_EDGE('',*,*,#4912,.T.);
#6569=ORIENTED_EDGE('',*,*,#4910,.F.);
#6570=ORIENTED_EDGE('',*,*,#4908,.T.);
#6571=ORIENTED_EDGE('',*,*,#4906,.F.);
#6572=ORIENTED_EDGE('',*,*,#4904,.T.);
#6573=ORIENTED_EDGE('',*,*,#4902,.F.);
#6574=ORIENTED_EDGE('',*,*,#4899,.T.);
#6575=ORIENTED_EDGE('',*,*,#4915,.F.);
#6576=ORIENTED_EDGE('',*,*,#4870,.T.);
#6577=ORIENTED_EDGE('',*,*,#4888,.T.);
#6578=ORIENTED_EDGE('',*,*,#4919,.T.);
#6579=ORIENTED_EDGE('',*,*,#4916,.T.);
#6580=ORIENTED_EDGE('',*,*,#4887,.F.);
#6581=ORIENTED_EDGE('',*,*,#4920,.F.);
#6582=ORIENTED_EDGE('',*,*,#4917,.F.);
#6583=ORIENTED_EDGE('',*,*,#4919,.F.);
#6584=ORIENTED_EDGE('',*,*,#4878,.T.);
#6585=ORIENTED_EDGE('',*,*,#4914,.T.);
#6586=ORIENTED_EDGE('',*,*,#4913,.T.);
#6587=ORIENTED_EDGE('',*,*,#4918,.T.);
#6588=ORIENTED_EDGE('',*,*,#4920,.T.);
#6589=ORIENTED_EDGE('',*,*,#4886,.T.);
#6590=ORIENTED_EDGE('',*,*,#4921,.F.);
#6591=ORIENTED_EDGE('',*,*,#4922,.T.);
#6592=ORIENTED_EDGE('',*,*,#4923,.F.);
#6593=ORIENTED_EDGE('',*,*,#4924,.T.);
#6594=ORIENTED_EDGE('',*,*,#4921,.T.);
#6595=ORIENTED_EDGE('',*,*,#4924,.F.);
#6596=ORIENTED_EDGE('',*,*,#4923,.T.);
#6597=ORIENTED_EDGE('',*,*,#4925,.F.);
#6598=ORIENTED_EDGE('',*,*,#4925,.T.);
#6599=ORIENTED_EDGE('',*,*,#4926,.T.);
#6600=ORIENTED_EDGE('',*,*,#4922,.F.);
#6601=ORIENTED_EDGE('',*,*,#4926,.F.);
#6602=ORIENTED_EDGE('',*,*,#4927,.F.);
#6603=ORIENTED_EDGE('',*,*,#4928,.T.);
#6604=ORIENTED_EDGE('',*,*,#4929,.F.);
#6605=ORIENTED_EDGE('',*,*,#4930,.T.);
#6606=ORIENTED_EDGE('',*,*,#4927,.T.);
#6607=ORIENTED_EDGE('',*,*,#4930,.F.);
#6608=ORIENTED_EDGE('',*,*,#4929,.T.);
#6609=ORIENTED_EDGE('',*,*,#4931,.F.);
#6610=ORIENTED_EDGE('',*,*,#4931,.T.);
#6611=ORIENTED_EDGE('',*,*,#4932,.T.);
#6612=ORIENTED_EDGE('',*,*,#4928,.F.);
#6613=ORIENTED_EDGE('',*,*,#4932,.F.);
#6614=ORIENTED_EDGE('',*,*,#4933,.F.);
#6615=ORIENTED_EDGE('',*,*,#4934,.F.);
#6616=ORIENTED_EDGE('',*,*,#4935,.T.);
#6617=ORIENTED_EDGE('',*,*,#4933,.T.);
#6618=ORIENTED_EDGE('',*,*,#4935,.F.);
#6619=ORIENTED_EDGE('',*,*,#4936,.F.);
#6620=ORIENTED_EDGE('',*,*,#4937,.T.);
#6621=ORIENTED_EDGE('',*,*,#4934,.T.);
#6622=ORIENTED_EDGE('',*,*,#4937,.F.);
#6623=ORIENTED_EDGE('',*,*,#4938,.F.);
#6624=ORIENTED_EDGE('',*,*,#4939,.T.);
#6625=ORIENTED_EDGE('',*,*,#4936,.T.);
#6626=ORIENTED_EDGE('',*,*,#4939,.F.);
#6627=ORIENTED_EDGE('',*,*,#4938,.T.);
#6628=ORIENTED_EDGE('',*,*,#4940,.F.);
#6629=ORIENTED_EDGE('',*,*,#4941,.F.);
#6630=ORIENTED_EDGE('',*,*,#4942,.T.);
#6631=ORIENTED_EDGE('',*,*,#4940,.T.);
#6632=ORIENTED_EDGE('',*,*,#4942,.F.);
#6633=ORIENTED_EDGE('',*,*,#4943,.F.);
#6634=ORIENTED_EDGE('',*,*,#4944,.T.);
#6635=ORIENTED_EDGE('',*,*,#4941,.T.);
#6636=ORIENTED_EDGE('',*,*,#4944,.F.);
#6637=ORIENTED_EDGE('',*,*,#4945,.F.);
#6638=ORIENTED_EDGE('',*,*,#4946,.T.);
#6639=ORIENTED_EDGE('',*,*,#4943,.T.);
#6640=ORIENTED_EDGE('',*,*,#4946,.F.);
#6641=ORIENTED_EDGE('',*,*,#4945,.T.);
#6642=ORIENTED_EDGE('',*,*,#4947,.T.);
#6643=ORIENTED_EDGE('',*,*,#4948,.T.);
#6644=ORIENTED_EDGE('',*,*,#4949,.T.);
#6645=ORIENTED_EDGE('',*,*,#4950,.F.);
#6646=ORIENTED_EDGE('',*,*,#4951,.T.);
#6647=ORIENTED_EDGE('',*,*,#4952,.T.);
#6648=ORIENTED_EDGE('',*,*,#4953,.T.);
#6649=ORIENTED_EDGE('',*,*,#4948,.F.);
#6650=ORIENTED_EDGE('',*,*,#4954,.T.);
#6651=ORIENTED_EDGE('',*,*,#4955,.T.);
#6652=ORIENTED_EDGE('',*,*,#4956,.T.);
#6653=ORIENTED_EDGE('',*,*,#4952,.F.);
#6654=ORIENTED_EDGE('',*,*,#4957,.T.);
#6655=ORIENTED_EDGE('',*,*,#4958,.T.);
#6656=ORIENTED_EDGE('',*,*,#4959,.T.);
#6657=ORIENTED_EDGE('',*,*,#4955,.F.);
#6658=ORIENTED_EDGE('',*,*,#4960,.T.);
#6659=ORIENTED_EDGE('',*,*,#4961,.T.);
#6660=ORIENTED_EDGE('',*,*,#4962,.T.);
#6661=ORIENTED_EDGE('',*,*,#4958,.F.);
#6662=ORIENTED_EDGE('',*,*,#4963,.T.);
#6663=ORIENTED_EDGE('',*,*,#4950,.T.);
#6664=ORIENTED_EDGE('',*,*,#4964,.T.);
#6665=ORIENTED_EDGE('',*,*,#4961,.F.);
#6666=ORIENTED_EDGE('',*,*,#4963,.F.);
#6667=ORIENTED_EDGE('',*,*,#4960,.F.);
#6668=ORIENTED_EDGE('',*,*,#4957,.F.);
#6669=ORIENTED_EDGE('',*,*,#4954,.F.);
#6670=ORIENTED_EDGE('',*,*,#4951,.F.);
#6671=ORIENTED_EDGE('',*,*,#4947,.F.);
#6672=ORIENTED_EDGE('',*,*,#4964,.F.);
#6673=ORIENTED_EDGE('',*,*,#4949,.F.);
#6674=ORIENTED_EDGE('',*,*,#4953,.F.);
#6675=ORIENTED_EDGE('',*,*,#4956,.F.);
#6676=ORIENTED_EDGE('',*,*,#4959,.F.);
#6677=ORIENTED_EDGE('',*,*,#4962,.F.);
#6678=ORIENTED_EDGE('',*,*,#4965,.T.);
#6679=ORIENTED_EDGE('',*,*,#4966,.T.);
#6680=ORIENTED_EDGE('',*,*,#4967,.T.);
#6681=ORIENTED_EDGE('',*,*,#4968,.F.);
#6682=ORIENTED_EDGE('',*,*,#4969,.T.);
#6683=ORIENTED_EDGE('',*,*,#4970,.T.);
#6684=ORIENTED_EDGE('',*,*,#4971,.T.);
#6685=ORIENTED_EDGE('',*,*,#4966,.F.);
#6686=ORIENTED_EDGE('',*,*,#4972,.T.);
#6687=ORIENTED_EDGE('',*,*,#4973,.T.);
#6688=ORIENTED_EDGE('',*,*,#4974,.T.);
#6689=ORIENTED_EDGE('',*,*,#4970,.F.);
#6690=ORIENTED_EDGE('',*,*,#4975,.T.);
#6691=ORIENTED_EDGE('',*,*,#4976,.T.);
#6692=ORIENTED_EDGE('',*,*,#4977,.T.);
#6693=ORIENTED_EDGE('',*,*,#4973,.F.);
#6694=ORIENTED_EDGE('',*,*,#4978,.T.);
#6695=ORIENTED_EDGE('',*,*,#4979,.T.);
#6696=ORIENTED_EDGE('',*,*,#4980,.T.);
#6697=ORIENTED_EDGE('',*,*,#4976,.F.);
#6698=ORIENTED_EDGE('',*,*,#4981,.T.);
#6699=ORIENTED_EDGE('',*,*,#4968,.T.);
#6700=ORIENTED_EDGE('',*,*,#4982,.T.);
#6701=ORIENTED_EDGE('',*,*,#4979,.F.);
#6702=ORIENTED_EDGE('',*,*,#4981,.F.);
#6703=ORIENTED_EDGE('',*,*,#4978,.F.);
#6704=ORIENTED_EDGE('',*,*,#4975,.F.);
#6705=ORIENTED_EDGE('',*,*,#4972,.F.);
#6706=ORIENTED_EDGE('',*,*,#4969,.F.);
#6707=ORIENTED_EDGE('',*,*,#4965,.F.);
#6708=ORIENTED_EDGE('',*,*,#4982,.F.);
#6709=ORIENTED_EDGE('',*,*,#4967,.F.);
#6710=ORIENTED_EDGE('',*,*,#4971,.F.);
#6711=ORIENTED_EDGE('',*,*,#4974,.F.);
#6712=ORIENTED_EDGE('',*,*,#4977,.F.);
#6713=ORIENTED_EDGE('',*,*,#4980,.F.);
#6714=ORIENTED_EDGE('',*,*,#4983,.F.);
#6715=ORIENTED_EDGE('',*,*,#4984,.F.);
#6716=ORIENTED_EDGE('',*,*,#4985,.F.);
#6717=ORIENTED_EDGE('',*,*,#4986,.T.);
#6718=ORIENTED_EDGE('',*,*,#4984,.T.);
#6719=ORIENTED_EDGE('',*,*,#4986,.F.);
#6720=ORIENTED_EDGE('',*,*,#4987,.F.);
#6721=ORIENTED_EDGE('',*,*,#4988,.T.);
#6722=ORIENTED_EDGE('',*,*,#4985,.T.);
#6723=ORIENTED_EDGE('',*,*,#4988,.F.);
#6724=ORIENTED_EDGE('',*,*,#4989,.F.);
#6725=ORIENTED_EDGE('',*,*,#4990,.T.);
#6726=ORIENTED_EDGE('',*,*,#4987,.T.);
#6727=ORIENTED_EDGE('',*,*,#4990,.F.);
#6728=ORIENTED_EDGE('',*,*,#4989,.T.);
#6729=ORIENTED_EDGE('',*,*,#4991,.F.);
#6730=ORIENTED_EDGE('',*,*,#4992,.F.);
#6731=ORIENTED_EDGE('',*,*,#4993,.T.);
#6732=ORIENTED_EDGE('',*,*,#4991,.T.);
#6733=ORIENTED_EDGE('',*,*,#4993,.F.);
#6734=ORIENTED_EDGE('',*,*,#4983,.T.);
#6735=ORIENTED_EDGE('',*,*,#4994,.T.);
#6736=ORIENTED_EDGE('',*,*,#4992,.T.);
#6737=ORIENTED_EDGE('',*,*,#4994,.F.);
#6738=ORIENTED_EDGE('',*,*,#4995,.F.);
#6739=ORIENTED_EDGE('',*,*,#4996,.T.);
#6740=ORIENTED_EDGE('',*,*,#4997,.F.);
#6741=ORIENTED_EDGE('',*,*,#4996,.F.);
#6742=ORIENTED_EDGE('',*,*,#4995,.T.);
#6743=ORIENTED_EDGE('',*,*,#4998,.F.);
#6744=ORIENTED_EDGE('',*,*,#4999,.T.);
#6745=ORIENTED_EDGE('',*,*,#5000,.T.);
#6746=ORIENTED_EDGE('',*,*,#4999,.F.);
#6747=ORIENTED_EDGE('',*,*,#5000,.F.);
#6748=ORIENTED_EDGE('',*,*,#5001,.F.);
#6749=ORIENTED_EDGE('',*,*,#5002,.T.);
#6750=ORIENTED_EDGE('',*,*,#5003,.T.);
#6751=ORIENTED_EDGE('',*,*,#5002,.F.);
#6752=ORIENTED_EDGE('',*,*,#5001,.T.);
#6753=ORIENTED_EDGE('',*,*,#4997,.T.);
#6754=ORIENTED_EDGE('',*,*,#5003,.F.);
#6755=ORIENTED_EDGE('',*,*,#4998,.T.);
#6756=ORIENTED_EDGE('',*,*,#5004,.F.);
#6757=ORIENTED_EDGE('',*,*,#5005,.T.);
#6758=ORIENTED_EDGE('',*,*,#5006,.T.);
#6759=ORIENTED_EDGE('',*,*,#5005,.F.);
#6760=ORIENTED_EDGE('',*,*,#5007,.F.);
#6761=ORIENTED_EDGE('',*,*,#5008,.T.);
#6762=ORIENTED_EDGE('',*,*,#5009,.T.);
#6763=ORIENTED_EDGE('',*,*,#5008,.F.);
#6764=ORIENTED_EDGE('',*,*,#5007,.T.);
#6765=ORIENTED_EDGE('',*,*,#5004,.T.);
#6766=ORIENTED_EDGE('',*,*,#5009,.F.);
#6767=ORIENTED_EDGE('',*,*,#5006,.F.);
#6768=ORIENTED_EDGE('',*,*,#5010,.F.);
#6769=ORIENTED_EDGE('',*,*,#5011,.T.);
#6770=ORIENTED_EDGE('',*,*,#5012,.T.);
#6771=ORIENTED_EDGE('',*,*,#5011,.F.);
#6772=ORIENTED_EDGE('',*,*,#5013,.F.);
#6773=ORIENTED_EDGE('',*,*,#5014,.T.);
#6774=ORIENTED_EDGE('',*,*,#5015,.T.);
#6775=ORIENTED_EDGE('',*,*,#5014,.F.);
#6776=ORIENTED_EDGE('',*,*,#5013,.T.);
#6777=ORIENTED_EDGE('',*,*,#5010,.T.);
#6778=ORIENTED_EDGE('',*,*,#5015,.F.);
#6779=ORIENTED_EDGE('',*,*,#5012,.F.);
#6780=ORIENTED_EDGE('',*,*,#5016,.F.);
#6781=ORIENTED_EDGE('',*,*,#5017,.T.);
#6782=ORIENTED_EDGE('',*,*,#5018,.F.);
#6783=ORIENTED_EDGE('',*,*,#5019,.F.);
#6784=ORIENTED_EDGE('',*,*,#5020,.T.);
#6785=ORIENTED_EDGE('',*,*,#5021,.F.);
#6786=ORIENTED_EDGE('',*,*,#5022,.F.);
#6787=ORIENTED_EDGE('',*,*,#5020,.F.);
#6788=ORIENTED_EDGE('',*,*,#5023,.F.);
#6789=ORIENTED_EDGE('',*,*,#5024,.F.);
#6790=ORIENTED_EDGE('',*,*,#5017,.F.);
#6791=ORIENTED_EDGE('',*,*,#5025,.F.);
#6792=ORIENTED_EDGE('',*,*,#5023,.T.);
#6793=ORIENTED_EDGE('',*,*,#5019,.T.);
#6794=ORIENTED_EDGE('',*,*,#5026,.F.);
#6795=ORIENTED_EDGE('',*,*,#5027,.T.);
#6796=ORIENTED_EDGE('',*,*,#5028,.T.);
#6797=ORIENTED_EDGE('',*,*,#5027,.F.);
#6798=ORIENTED_EDGE('',*,*,#5024,.T.);
#6799=ORIENTED_EDGE('',*,*,#5025,.T.);
#6800=ORIENTED_EDGE('',*,*,#5018,.T.);
#6801=ORIENTED_EDGE('',*,*,#5016,.T.);
#6802=ORIENTED_EDGE('',*,*,#5029,.F.);
#6803=ORIENTED_EDGE('',*,*,#5030,.T.);
#6804=ORIENTED_EDGE('',*,*,#5031,.T.);
#6805=ORIENTED_EDGE('',*,*,#5030,.F.);
#6806=ORIENTED_EDGE('',*,*,#5021,.T.);
#6807=ORIENTED_EDGE('',*,*,#5022,.T.);
#6808=ORIENTED_EDGE('',*,*,#5029,.T.);
#6809=ORIENTED_EDGE('',*,*,#5026,.T.);
#6810=ORIENTED_EDGE('',*,*,#5031,.F.);
#6811=ORIENTED_EDGE('',*,*,#5028,.F.);
#6812=ORIENTED_EDGE('',*,*,#5032,.F.);
#6813=ORIENTED_EDGE('',*,*,#5033,.T.);
#6814=ORIENTED_EDGE('',*,*,#5034,.F.);
#6815=ORIENTED_EDGE('',*,*,#5035,.F.);
#6816=ORIENTED_EDGE('',*,*,#5036,.T.);
#6817=ORIENTED_EDGE('',*,*,#5037,.F.);
#6818=ORIENTED_EDGE('',*,*,#5038,.F.);
#6819=ORIENTED_EDGE('',*,*,#5036,.F.);
#6820=ORIENTED_EDGE('',*,*,#5039,.F.);
#6821=ORIENTED_EDGE('',*,*,#5040,.F.);
#6822=ORIENTED_EDGE('',*,*,#5033,.F.);
#6823=ORIENTED_EDGE('',*,*,#5041,.F.);
#6824=ORIENTED_EDGE('',*,*,#5039,.T.);
#6825=ORIENTED_EDGE('',*,*,#5035,.T.);
#6826=ORIENTED_EDGE('',*,*,#5042,.F.);
#6827=ORIENTED_EDGE('',*,*,#5043,.T.);
#6828=ORIENTED_EDGE('',*,*,#5044,.T.);
#6829=ORIENTED_EDGE('',*,*,#5043,.F.);
#6830=ORIENTED_EDGE('',*,*,#5040,.T.);
#6831=ORIENTED_EDGE('',*,*,#5041,.T.);
#6832=ORIENTED_EDGE('',*,*,#5034,.T.);
#6833=ORIENTED_EDGE('',*,*,#5032,.T.);
#6834=ORIENTED_EDGE('',*,*,#5045,.F.);
#6835=ORIENTED_EDGE('',*,*,#5046,.T.);
#6836=ORIENTED_EDGE('',*,*,#5047,.T.);
#6837=ORIENTED_EDGE('',*,*,#5046,.F.);
#6838=ORIENTED_EDGE('',*,*,#5037,.T.);
#6839=ORIENTED_EDGE('',*,*,#5038,.T.);
#6840=ORIENTED_EDGE('',*,*,#5045,.T.);
#6841=ORIENTED_EDGE('',*,*,#5042,.T.);
#6842=ORIENTED_EDGE('',*,*,#5047,.F.);
#6843=ORIENTED_EDGE('',*,*,#5044,.F.);
#6844=ORIENTED_EDGE('',*,*,#5048,.F.);
#6845=ORIENTED_EDGE('',*,*,#5049,.T.);
#6846=ORIENTED_EDGE('',*,*,#5050,.T.);
#6847=ORIENTED_EDGE('',*,*,#5049,.F.);
#6848=ORIENTED_EDGE('',*,*,#5051,.F.);
#6849=ORIENTED_EDGE('',*,*,#5052,.T.);
#6850=ORIENTED_EDGE('',*,*,#5053,.T.);
#6851=ORIENTED_EDGE('',*,*,#5052,.F.);
#6852=ORIENTED_EDGE('',*,*,#5051,.T.);
#6853=ORIENTED_EDGE('',*,*,#5048,.T.);
#6854=ORIENTED_EDGE('',*,*,#5053,.F.);
#6855=ORIENTED_EDGE('',*,*,#5050,.F.);
#6856=ORIENTED_EDGE('',*,*,#5054,.F.);
#6857=ORIENTED_EDGE('',*,*,#5055,.T.);
#6858=ORIENTED_EDGE('',*,*,#5056,.T.);
#6859=ORIENTED_EDGE('',*,*,#5055,.F.);
#6860=ORIENTED_EDGE('',*,*,#5057,.F.);
#6861=ORIENTED_EDGE('',*,*,#5058,.T.);
#6862=ORIENTED_EDGE('',*,*,#5059,.T.);
#6863=ORIENTED_EDGE('',*,*,#5058,.F.);
#6864=ORIENTED_EDGE('',*,*,#5057,.T.);
#6865=ORIENTED_EDGE('',*,*,#5054,.T.);
#6866=ORIENTED_EDGE('',*,*,#5059,.F.);
#6867=ORIENTED_EDGE('',*,*,#5056,.F.);
#6868=ORIENTED_EDGE('',*,*,#5060,.F.);
#6869=ORIENTED_EDGE('',*,*,#5061,.T.);
#6870=ORIENTED_EDGE('',*,*,#5062,.F.);
#6871=ORIENTED_EDGE('',*,*,#5063,.F.);
#6872=ORIENTED_EDGE('',*,*,#5064,.T.);
#6873=ORIENTED_EDGE('',*,*,#5065,.F.);
#6874=ORIENTED_EDGE('',*,*,#5066,.F.);
#6875=ORIENTED_EDGE('',*,*,#5064,.F.);
#6876=ORIENTED_EDGE('',*,*,#5067,.F.);
#6877=ORIENTED_EDGE('',*,*,#5068,.F.);
#6878=ORIENTED_EDGE('',*,*,#5061,.F.);
#6879=ORIENTED_EDGE('',*,*,#5069,.F.);
#6880=ORIENTED_EDGE('',*,*,#5067,.T.);
#6881=ORIENTED_EDGE('',*,*,#5063,.T.);
#6882=ORIENTED_EDGE('',*,*,#5070,.F.);
#6883=ORIENTED_EDGE('',*,*,#5071,.T.);
#6884=ORIENTED_EDGE('',*,*,#5072,.T.);
#6885=ORIENTED_EDGE('',*,*,#5071,.F.);
#6886=ORIENTED_EDGE('',*,*,#5068,.T.);
#6887=ORIENTED_EDGE('',*,*,#5069,.T.);
#6888=ORIENTED_EDGE('',*,*,#5062,.T.);
#6889=ORIENTED_EDGE('',*,*,#5060,.T.);
#6890=ORIENTED_EDGE('',*,*,#5073,.F.);
#6891=ORIENTED_EDGE('',*,*,#5074,.T.);
#6892=ORIENTED_EDGE('',*,*,#5075,.T.);
#6893=ORIENTED_EDGE('',*,*,#5074,.F.);
#6894=ORIENTED_EDGE('',*,*,#5065,.T.);
#6895=ORIENTED_EDGE('',*,*,#5066,.T.);
#6896=ORIENTED_EDGE('',*,*,#5073,.T.);
#6897=ORIENTED_EDGE('',*,*,#5070,.T.);
#6898=ORIENTED_EDGE('',*,*,#5075,.F.);
#6899=ORIENTED_EDGE('',*,*,#5072,.F.);
#6900=ORIENTED_EDGE('',*,*,#5076,.F.);
#6901=ORIENTED_EDGE('',*,*,#5077,.T.);
#6902=ORIENTED_EDGE('',*,*,#5078,.F.);
#6903=ORIENTED_EDGE('',*,*,#5079,.F.);
#6904=ORIENTED_EDGE('',*,*,#5080,.T.);
#6905=ORIENTED_EDGE('',*,*,#5081,.F.);
#6906=ORIENTED_EDGE('',*,*,#5082,.F.);
#6907=ORIENTED_EDGE('',*,*,#5080,.F.);
#6908=ORIENTED_EDGE('',*,*,#5083,.F.);
#6909=ORIENTED_EDGE('',*,*,#5084,.F.);
#6910=ORIENTED_EDGE('',*,*,#5077,.F.);
#6911=ORIENTED_EDGE('',*,*,#5085,.F.);
#6912=ORIENTED_EDGE('',*,*,#5083,.T.);
#6913=ORIENTED_EDGE('',*,*,#5079,.T.);
#6914=ORIENTED_EDGE('',*,*,#5086,.F.);
#6915=ORIENTED_EDGE('',*,*,#5087,.T.);
#6916=ORIENTED_EDGE('',*,*,#5088,.T.);
#6917=ORIENTED_EDGE('',*,*,#5087,.F.);
#6918=ORIENTED_EDGE('',*,*,#5084,.T.);
#6919=ORIENTED_EDGE('',*,*,#5085,.T.);
#6920=ORIENTED_EDGE('',*,*,#5078,.T.);
#6921=ORIENTED_EDGE('',*,*,#5076,.T.);
#6922=ORIENTED_EDGE('',*,*,#5089,.F.);
#6923=ORIENTED_EDGE('',*,*,#5090,.T.);
#6924=ORIENTED_EDGE('',*,*,#5091,.T.);
#6925=ORIENTED_EDGE('',*,*,#5090,.F.);
#6926=ORIENTED_EDGE('',*,*,#5081,.T.);
#6927=ORIENTED_EDGE('',*,*,#5082,.T.);
#6928=ORIENTED_EDGE('',*,*,#5089,.T.);
#6929=ORIENTED_EDGE('',*,*,#5086,.T.);
#6930=ORIENTED_EDGE('',*,*,#5091,.F.);
#6931=ORIENTED_EDGE('',*,*,#5088,.F.);
#6932=ORIENTED_EDGE('',*,*,#5092,.F.);
#6933=ORIENTED_EDGE('',*,*,#5093,.T.);
#6934=ORIENTED_EDGE('',*,*,#5094,.F.);
#6935=ORIENTED_EDGE('',*,*,#5095,.F.);
#6936=ORIENTED_EDGE('',*,*,#5096,.T.);
#6937=ORIENTED_EDGE('',*,*,#5097,.F.);
#6938=ORIENTED_EDGE('',*,*,#5098,.F.);
#6939=ORIENTED_EDGE('',*,*,#5096,.F.);
#6940=ORIENTED_EDGE('',*,*,#5099,.F.);
#6941=ORIENTED_EDGE('',*,*,#5100,.F.);
#6942=ORIENTED_EDGE('',*,*,#5093,.F.);
#6943=ORIENTED_EDGE('',*,*,#5101,.F.);
#6944=ORIENTED_EDGE('',*,*,#5099,.T.);
#6945=ORIENTED_EDGE('',*,*,#5095,.T.);
#6946=ORIENTED_EDGE('',*,*,#5102,.F.);
#6947=ORIENTED_EDGE('',*,*,#5103,.T.);
#6948=ORIENTED_EDGE('',*,*,#5104,.F.);
#6949=ORIENTED_EDGE('',*,*,#5103,.F.);
#6950=ORIENTED_EDGE('',*,*,#5105,.F.);
#6951=ORIENTED_EDGE('',*,*,#5106,.T.);
#6952=ORIENTED_EDGE('',*,*,#5107,.F.);
#6953=ORIENTED_EDGE('',*,*,#5106,.F.);
#6954=ORIENTED_EDGE('',*,*,#5108,.F.);
#6955=ORIENTED_EDGE('',*,*,#5109,.T.);
#6956=ORIENTED_EDGE('',*,*,#5110,.F.);
#6957=ORIENTED_EDGE('',*,*,#5109,.F.);
#6958=ORIENTED_EDGE('',*,*,#5111,.F.);
#6959=ORIENTED_EDGE('',*,*,#5112,.T.);
#6960=ORIENTED_EDGE('',*,*,#5113,.F.);
#6961=ORIENTED_EDGE('',*,*,#5112,.F.);
#6962=ORIENTED_EDGE('',*,*,#5114,.T.);
#6963=ORIENTED_EDGE('',*,*,#5115,.F.);
#6964=ORIENTED_EDGE('',*,*,#5113,.T.);
#6965=ORIENTED_EDGE('',*,*,#5110,.T.);
#6966=ORIENTED_EDGE('',*,*,#5107,.T.);
#6967=ORIENTED_EDGE('',*,*,#5104,.T.);
#6968=ORIENTED_EDGE('',*,*,#5114,.F.);
#6969=ORIENTED_EDGE('',*,*,#5116,.T.);
#6970=ORIENTED_EDGE('',*,*,#5117,.T.);
#6971=ORIENTED_EDGE('',*,*,#5116,.F.);
#6972=ORIENTED_EDGE('',*,*,#5118,.F.);
#6973=ORIENTED_EDGE('',*,*,#5119,.T.);
#6974=ORIENTED_EDGE('',*,*,#5120,.T.);
#6975=ORIENTED_EDGE('',*,*,#5119,.F.);
#6976=ORIENTED_EDGE('',*,*,#5100,.T.);
#6977=ORIENTED_EDGE('',*,*,#5101,.T.);
#6978=ORIENTED_EDGE('',*,*,#5094,.T.);
#6979=ORIENTED_EDGE('',*,*,#5092,.T.);
#6980=ORIENTED_EDGE('',*,*,#5121,.F.);
#6981=ORIENTED_EDGE('',*,*,#5122,.T.);
#6982=ORIENTED_EDGE('',*,*,#5115,.T.);
#6983=ORIENTED_EDGE('',*,*,#5122,.F.);
#6984=ORIENTED_EDGE('',*,*,#5097,.T.);
#6985=ORIENTED_EDGE('',*,*,#5098,.T.);
#6986=ORIENTED_EDGE('',*,*,#5121,.T.);
#6987=ORIENTED_EDGE('',*,*,#5118,.T.);
#6988=ORIENTED_EDGE('',*,*,#5117,.F.);
#6989=ORIENTED_EDGE('',*,*,#5120,.F.);
#6990=ORIENTED_EDGE('',*,*,#5111,.T.);
#6991=ORIENTED_EDGE('',*,*,#5108,.T.);
#6992=ORIENTED_EDGE('',*,*,#5105,.T.);
#6993=ORIENTED_EDGE('',*,*,#5102,.T.);
#6994=ORIENTED_EDGE('',*,*,#5123,.F.);
#6995=ORIENTED_EDGE('',*,*,#5124,.T.);
#6996=ORIENTED_EDGE('',*,*,#5125,.T.);
#6997=ORIENTED_EDGE('',*,*,#5126,.F.);
#6998=ORIENTED_EDGE('',*,*,#5127,.F.);
#6999=ORIENTED_EDGE('',*,*,#5128,.T.);
#7000=ORIENTED_EDGE('',*,*,#5129,.T.);
#7001=ORIENTED_EDGE('',*,*,#5124,.F.);
#7002=ORIENTED_EDGE('',*,*,#5130,.F.);
#7003=ORIENTED_EDGE('',*,*,#5131,.T.);
#7004=ORIENTED_EDGE('',*,*,#5132,.T.);
#7005=ORIENTED_EDGE('',*,*,#5128,.F.);
#7006=ORIENTED_EDGE('',*,*,#5133,.F.);
#7007=ORIENTED_EDGE('',*,*,#5134,.T.);
#7008=ORIENTED_EDGE('',*,*,#5135,.T.);
#7009=ORIENTED_EDGE('',*,*,#5131,.F.);
#7010=ORIENTED_EDGE('',*,*,#5136,.F.);
#7011=ORIENTED_EDGE('',*,*,#5137,.T.);
#7012=ORIENTED_EDGE('',*,*,#5138,.T.);
#7013=ORIENTED_EDGE('',*,*,#5134,.F.);
#7014=ORIENTED_EDGE('',*,*,#5139,.F.);
#7015=ORIENTED_EDGE('',*,*,#5126,.T.);
#7016=ORIENTED_EDGE('',*,*,#5140,.T.);
#7017=ORIENTED_EDGE('',*,*,#5137,.F.);
#7018=ORIENTED_EDGE('',*,*,#5140,.F.);
#7019=ORIENTED_EDGE('',*,*,#5125,.F.);
#7020=ORIENTED_EDGE('',*,*,#5129,.F.);
#7021=ORIENTED_EDGE('',*,*,#5132,.F.);
#7022=ORIENTED_EDGE('',*,*,#5135,.F.);
#7023=ORIENTED_EDGE('',*,*,#5138,.F.);
#7024=ORIENTED_EDGE('',*,*,#5141,.F.);
#7025=ORIENTED_EDGE('',*,*,#5123,.T.);
#7026=ORIENTED_EDGE('',*,*,#5139,.T.);
#7027=ORIENTED_EDGE('',*,*,#5136,.T.);
#7028=ORIENTED_EDGE('',*,*,#5133,.T.);
#7029=ORIENTED_EDGE('',*,*,#5130,.T.);
#7030=ORIENTED_EDGE('',*,*,#5127,.T.);
#7031=ORIENTED_EDGE('',*,*,#5142,.F.);
#7032=ORIENTED_EDGE('',*,*,#5143,.T.);
#7033=ORIENTED_EDGE('',*,*,#5141,.T.);
#7034=ORIENTED_EDGE('',*,*,#5143,.F.);
#7035=ORIENTED_EDGE('',*,*,#5144,.F.);
#7036=ORIENTED_EDGE('',*,*,#5145,.T.);
#7037=ORIENTED_EDGE('',*,*,#5142,.T.);
#7038=ORIENTED_EDGE('',*,*,#5145,.F.);
#7039=ORIENTED_EDGE('',*,*,#5146,.F.);
#7040=ORIENTED_EDGE('',*,*,#5147,.T.);
#7041=ORIENTED_EDGE('',*,*,#5144,.T.);
#7042=ORIENTED_EDGE('',*,*,#5147,.F.);
#7043=ORIENTED_EDGE('',*,*,#5146,.T.);
#7044=CYLINDRICAL_SURFACE('',#8145,0.165);
#7045=CYLINDRICAL_SURFACE('',#8148,0.165);
#7046=CYLINDRICAL_SURFACE('',#8151,0.165);
#7047=CYLINDRICAL_SURFACE('',#8154,0.165);
#7048=CYLINDRICAL_SURFACE('',#8157,0.210000000000001);
#7049=CYLINDRICAL_SURFACE('',#8160,0.210000000000001);
#7050=CYLINDRICAL_SURFACE('',#8163,0.210000000000001);
#7051=CYLINDRICAL_SURFACE('',#8166,0.210000000000001);
#7052=CYLINDRICAL_SURFACE('',#8169,0.25);
#7053=CYLINDRICAL_SURFACE('',#8172,0.25);
#7054=CYLINDRICAL_SURFACE('',#8175,0.25);
#7055=CYLINDRICAL_SURFACE('',#8178,0.25);
#7056=CYLINDRICAL_SURFACE('',#8188,0.165);
#7057=CYLINDRICAL_SURFACE('',#8191,0.165);
#7058=CYLINDRICAL_SURFACE('',#8194,0.165);
#7059=CYLINDRICAL_SURFACE('',#8197,0.165);
#7060=CYLINDRICAL_SURFACE('',#8202,0.6);
#7061=CYLINDRICAL_SURFACE('',#8211,0.6);
#7062=CYLINDRICAL_SURFACE('',#8216,0.33);
#7063=CYLINDRICAL_SURFACE('',#8218,0.33);
#7064=CYLINDRICAL_SURFACE('',#8228,1.6);
#7065=CYLINDRICAL_SURFACE('',#8230,2.5);
#7066=CYLINDRICAL_SURFACE('',#8234,0.225);
#7067=CYLINDRICAL_SURFACE('',#8237,0.225);
#7068=CYLINDRICAL_SURFACE('',#8240,0.225);
#7069=CYLINDRICAL_SURFACE('',#8243,0.225);
#7070=CYLINDRICAL_SURFACE('',#8246,1.59);
#7071=CYLINDRICAL_SURFACE('',#8251,1.1);
#7072=CYLINDRICAL_SURFACE('',#8253,2.5);
#7073=CYLINDRICAL_SURFACE('',#8259,0.225);
#7074=CYLINDRICAL_SURFACE('',#8262,0.225);
#7075=CYLINDRICAL_SURFACE('',#8265,0.225);
#7076=CYLINDRICAL_SURFACE('',#8268,0.225);
#7077=CYLINDRICAL_SURFACE('',#8271,1.59);
#7078=CYLINDRICAL_SURFACE('',#8276,1.1);
#7079=CYLINDRICAL_SURFACE('',#8278,2.5);
#7080=CYLINDRICAL_SURFACE('',#8284,0.165);
#7081=CYLINDRICAL_SURFACE('',#8287,0.165);
#7082=CYLINDRICAL_SURFACE('',#8290,0.165);
#7083=CYLINDRICAL_SURFACE('',#8293,0.165);
#7084=CYLINDRICAL_SURFACE('',#8298,0.6);
#7085=CYLINDRICAL_SURFACE('',#8307,0.6);
#7086=CYLINDRICAL_SURFACE('',#8312,0.33);
#7087=CYLINDRICAL_SURFACE('',#8314,0.33);
#7088=CYLINDRICAL_SURFACE('',#8324,1.6);
#7089=CYLINDRICAL_SURFACE('',#8326,2.5);
#7090=CYLINDRICAL_SURFACE('',#8330,0.225);
#7091=CYLINDRICAL_SURFACE('',#8333,0.225);
#7092=CYLINDRICAL_SURFACE('',#8336,0.225);
#7093=CYLINDRICAL_SURFACE('',#8339,0.225);
#7094=CYLINDRICAL_SURFACE('',#8342,1.59);
#7095=CYLINDRICAL_SURFACE('',#8347,1.1);
#7096=CYLINDRICAL_SURFACE('',#8349,2.5);
#7097=CYLINDRICAL_SURFACE('',#8355,0.225);
#7098=CYLINDRICAL_SURFACE('',#8358,0.225);
#7099=CYLINDRICAL_SURFACE('',#8361,0.225);
#7100=CYLINDRICAL_SURFACE('',#8364,0.225);
#7101=CYLINDRICAL_SURFACE('',#8367,1.59);
#7102=CYLINDRICAL_SURFACE('',#8372,1.1);
#7103=CYLINDRICAL_SURFACE('',#8374,2.5);
#7104=CYLINDRICAL_SURFACE('',#8380,0.165);
#7105=CYLINDRICAL_SURFACE('',#8383,0.165);
#7106=CYLINDRICAL_SURFACE('',#8386,0.165);
#7107=CYLINDRICAL_SURFACE('',#8389,0.165);
#7108=CYLINDRICAL_SURFACE('',#8399,2.35);
#7109=CYLINDRICAL_SURFACE('',#8402,3.);
#7110=CYLINDRICAL_SURFACE('',#8408,0.225);
#7111=CYLINDRICAL_SURFACE('',#8411,0.225);
#7112=CYLINDRICAL_SURFACE('',#8414,0.225);
#7113=CYLINDRICAL_SURFACE('',#8417,0.225);
#7114=CYLINDRICAL_SURFACE('',#8420,2.34);
#7115=CYLINDRICAL_SURFACE('',#8425,1.9);
#7116=CYLINDRICAL_SURFACE('',#8427,3.);
#7117=CYLINDRICAL_SURFACE('',#8433,0.225);
#7118=CYLINDRICAL_SURFACE('',#8436,0.225);
#7119=CYLINDRICAL_SURFACE('',#8439,0.225);
#7120=CYLINDRICAL_SURFACE('',#8442,0.225);
#7121=CYLINDRICAL_SURFACE('',#8445,2.34);
#7122=CYLINDRICAL_SURFACE('',#8450,1.9);
#7123=CYLINDRICAL_SURFACE('',#8452,3.);
#7124=CYLINDRICAL_SURFACE('',#8458,0.164999999999999);
#7125=CYLINDRICAL_SURFACE('',#8462,0.164999999999999);
#7126=CYLINDRICAL_SURFACE('',#8466,0.5);
#7127=CYLINDRICAL_SURFACE('',#8471,0.5);
#7128=CYLINDRICAL_SURFACE('',#8476,0.5);
#7129=CYLINDRICAL_SURFACE('',#8481,0.5);
#7130=CYLINDRICAL_SURFACE('',#8486,0.275);
#7131=CYLINDRICAL_SURFACE('',#8488,0.275);
#7132=CYLINDRICAL_SURFACE('',#8490,0.275);
#7133=CYLINDRICAL_SURFACE('',#8492,0.275);
#7134=CYLINDRICAL_SURFACE('',#8501,0.225);
#7135=CYLINDRICAL_SURFACE('',#8504,0.225);
#7136=CYLINDRICAL_SURFACE('',#8518,0.4);
#7137=CYLINDRICAL_SURFACE('',#8523,0.225);
#7138=CYLINDRICAL_SURFACE('',#8527,0.9);
#7139=CYLINDRICAL_SURFACE('',#8531,0.4);
#7140=CYLINDRICAL_SURFACE('',#8536,0.225);
#7141=CYLINDRICAL_SURFACE('',#8540,0.9);
#7142=CYLINDRICAL_SURFACE('',#8544,0.4);
#7143=CYLINDRICAL_SURFACE('',#8549,0.225);
#7144=CYLINDRICAL_SURFACE('',#8553,0.9);
#7145=CYLINDRICAL_SURFACE('',#8557,0.4);
#7146=CYLINDRICAL_SURFACE('',#8562,0.225);
#7147=CYLINDRICAL_SURFACE('',#8566,0.9);
#7148=CYLINDRICAL_SURFACE('',#8613,0.5);
#7149=CYLINDRICAL_SURFACE('',#8621,0.2942);
#7150=CYLINDRICAL_SURFACE('',#8630,1.070235);
#7151=CYLINDRICAL_SURFACE('',#8632,0.6);
#7152=CYLINDRICAL_SURFACE('',#8638,1.070235);
#7153=CYLINDRICAL_SURFACE('',#8650,1.129765);
#7154=CYLINDRICAL_SURFACE('',#8657,1.6);
#7155=CYLINDRICAL_SURFACE('',#8662,1.129765);
#7156=CYLINDRICAL_SURFACE('',#8682,1.123812);
#7157=CYLINDRICAL_SURFACE('',#8718,1.076188);
#7158=CYLINDRICAL_SURFACE('',#8732,1.119765);
#7159=CYLINDRICAL_SURFACE('',#8736,1.085235);
#7160=CYLINDRICAL_SURFACE('',#8740,1.119765);
#7161=CYLINDRICAL_SURFACE('',#8744,1.085235);
#7162=CYLINDRICAL_SURFACE('',#8758,1.63531);
#7163=CYLINDRICAL_SURFACE('',#8760,1.);
#7164=CYLINDRICAL_SURFACE('',#8766,1.63531);
#7165=CYLINDRICAL_SURFACE('',#8778,1.71469);
#7166=CYLINDRICAL_SURFACE('',#8785,2.35);
#7167=CYLINDRICAL_SURFACE('',#8790,1.71469);
#7168=CYLINDRICAL_SURFACE('',#8812,1.706752);
#7169=CYLINDRICAL_SURFACE('',#8852,1.643248);
#7170=CYLINDRICAL_SURFACE('',#8866,1.70469);
#7171=CYLINDRICAL_SURFACE('',#8870,1.65031);
#7172=CYLINDRICAL_SURFACE('',#8874,1.70469);
#7173=CYLINDRICAL_SURFACE('',#8878,1.65031);
#7174=CYLINDRICAL_SURFACE('',#8889,0.425);
#7175=CYLINDRICAL_SURFACE('',#8897,0.24505);
#7176=CYLINDRICAL_SURFACE('',#8925,0.35);
#7177=CYLINDRICAL_SURFACE('',#8933,0.1954);
#7178=CYLINDRICAL_SURFACE('',#8992,0.6);
#7179=CYLINDRICAL_SURFACE('',#8996,0.6);
#7180=CYLINDRICAL_SURFACE('',#9000,1.);
#7181=CYLINDRICAL_SURFACE('',#9006,0.605);
#7182=CYLINDRICAL_SURFACE('',#9009,0.9);
#7183=CYLINDRICAL_SURFACE('',#9015,0.605);
#7184=CYLINDRICAL_SURFACE('',#9018,0.9);
#7185=CYLINDRICAL_SURFACE('',#9026,0.21);
#7186=CYLINDRICAL_SURFACE('',#9030,0.605);
#7187=CYLINDRICAL_SURFACE('',#9033,1.);
#7188=CYLINDRICAL_SURFACE('',#9041,0.21);
#7189=CYLINDRICAL_SURFACE('',#9045,0.605);
#7190=CYLINDRICAL_SURFACE('',#9048,1.);
#7191=CYLINDRICAL_SURFACE('',#9054,0.605);
#7192=CYLINDRICAL_SURFACE('',#9057,0.9);
#7193=CYLINDRICAL_SURFACE('',#9063,0.605);
#7194=CYLINDRICAL_SURFACE('',#9066,0.9);
#7195=CYLINDRICAL_SURFACE('',#9074,0.21);
#7196=CYLINDRICAL_SURFACE('',#9078,1.005);
#7197=CYLINDRICAL_SURFACE('',#9081,1.5);
#7198=CYLINDRICAL_SURFACE('',#9089,0.21);
#7199=CYLINDRICAL_SURFACE('',#9093,1.005);
#7200=CYLINDRICAL_SURFACE('',#9096,1.5);
#7201=CYLINDRICAL_SURFACE('',#9104,0.21);
#7202=CYLINDRICAL_SURFACE('',#9108,0.225);
#7203=CYLINDRICAL_SURFACE('',#9111,0.225);
#7204=CYLINDRICAL_SURFACE('',#9114,0.225);
#7205=CYLINDRICAL_SURFACE('',#9117,0.225);
#7206=CYLINDRICAL_SURFACE('',#9123,2.3);
#7207=CYLINDRICAL_SURFACE('',#9125,0.6);
#7208=CYLINDRICAL_SURFACE('',#9128,1.5);
#7209=CYLINDRICAL_SURFACE('',#9144,0.24505);
#7210=ADVANCED_FACE('',(#1099),#7044,.F.);
#7211=ADVANCED_FACE('',(#1100),#7045,.F.);
#7212=ADVANCED_FACE('',(#1101),#7046,.F.);
#7213=ADVANCED_FACE('',(#1102),#7047,.F.);
#7214=ADVANCED_FACE('',(#1103),#7048,.F.);
#7215=ADVANCED_FACE('',(#1104),#7049,.F.);
#7216=ADVANCED_FACE('',(#1105),#7050,.F.);
#7217=ADVANCED_FACE('',(#1106),#7051,.F.);
#7218=ADVANCED_FACE('',(#1107),#7052,.F.);
#7219=ADVANCED_FACE('',(#1108),#7053,.F.);
#7220=ADVANCED_FACE('',(#1109),#7054,.F.);
#7221=ADVANCED_FACE('',(#1110),#7055,.F.);
#7222=ADVANCED_FACE('',(#1111),#874,.T.);
#7223=ADVANCED_FACE('',(#1112),#875,.T.);
#7224=ADVANCED_FACE('',(#1113),#876,.T.);
#7225=ADVANCED_FACE('',(#1114),#877,.T.);
#7226=ADVANCED_FACE('',(#1115,#644,#645,#646,#647,#648,#649,#650,#651,#652,
#653,#654,#655),#878,.T.);
#7227=ADVANCED_FACE('',(#1116,#656,#657,#658,#659,#660,#661,#662,#663,#664,
#665,#666,#667),#879,.F.);
#7228=ADVANCED_FACE('',(#1117),#7056,.F.);
#7229=ADVANCED_FACE('',(#1118),#7057,.F.);
#7230=ADVANCED_FACE('',(#1119),#7058,.F.);
#7231=ADVANCED_FACE('',(#1120),#7059,.F.);
#7232=ADVANCED_FACE('',(#1121),#880,.F.);
#7233=ADVANCED_FACE('',(#1122),#7060,.F.);
#7234=ADVANCED_FACE('',(#1123,#668),#881,.T.);
#7235=ADVANCED_FACE('',(#1124),#882,.F.);
#7236=ADVANCED_FACE('',(#1125),#7061,.F.);
#7237=ADVANCED_FACE('',(#1126,#669),#883,.T.);
#7238=ADVANCED_FACE('',(#1127),#7062,.F.);
#7239=ADVANCED_FACE('',(#1128),#7063,.F.);
#7240=ADVANCED_FACE('',(#1129,#670),#884,.T.);
#7241=ADVANCED_FACE('',(#1130,#671),#885,.T.);
#7242=ADVANCED_FACE('',(#1131),#886,.T.);
#7243=ADVANCED_FACE('',(#1132,#672,#673),#887,.T.);
#7244=ADVANCED_FACE('',(#1133),#888,.T.);
#7245=ADVANCED_FACE('',(#1134,#674,#675,#676,#677,#678),#889,.T.);
#7246=ADVANCED_FACE('',(#1135),#7064,.F.);
#7247=ADVANCED_FACE('',(#1136),#7065,.T.);
#7248=ADVANCED_FACE('',(#1137,#679,#680,#681,#682,#683),#890,.F.);
#7249=ADVANCED_FACE('',(#1138),#7066,.F.);
#7250=ADVANCED_FACE('',(#1139),#7067,.F.);
#7251=ADVANCED_FACE('',(#1140),#7068,.F.);
#7252=ADVANCED_FACE('',(#1141),#7069,.F.);
#7253=ADVANCED_FACE('',(#1142),#7070,.T.);
#7254=ADVANCED_FACE('',(#1143,#684),#891,.T.);
#7255=ADVANCED_FACE('',(#1144),#7071,.F.);
#7256=ADVANCED_FACE('',(#1145),#7072,.T.);
#7257=ADVANCED_FACE('',(#1146,#685,#686,#687,#688,#689),#892,.T.);
#7258=ADVANCED_FACE('',(#1147,#690,#691,#692,#693,#694),#893,.F.);
#7259=ADVANCED_FACE('',(#1148),#7073,.F.);
#7260=ADVANCED_FACE('',(#1149),#7074,.F.);
#7261=ADVANCED_FACE('',(#1150),#7075,.F.);
#7262=ADVANCED_FACE('',(#1151),#7076,.F.);
#7263=ADVANCED_FACE('',(#1152),#7077,.T.);
#7264=ADVANCED_FACE('',(#1153,#695),#894,.F.);
#7265=ADVANCED_FACE('',(#1154),#7078,.F.);
#7266=ADVANCED_FACE('',(#1155),#7079,.T.);
#7267=ADVANCED_FACE('',(#1156,#696,#697,#698,#699,#700),#895,.T.);
#7268=ADVANCED_FACE('',(#1157,#701,#702,#703,#704,#705),#896,.F.);
#7269=ADVANCED_FACE('',(#1158),#7080,.F.);
#7270=ADVANCED_FACE('',(#1159),#7081,.F.);
#7271=ADVANCED_FACE('',(#1160),#7082,.F.);
#7272=ADVANCED_FACE('',(#1161),#7083,.F.);
#7273=ADVANCED_FACE('',(#1162),#897,.F.);
#7274=ADVANCED_FACE('',(#1163),#7084,.F.);
#7275=ADVANCED_FACE('',(#1164,#706),#898,.T.);
#7276=ADVANCED_FACE('',(#1165),#899,.F.);
#7277=ADVANCED_FACE('',(#1166),#7085,.F.);
#7278=ADVANCED_FACE('',(#1167,#707),#900,.T.);
#7279=ADVANCED_FACE('',(#1168),#7086,.F.);
#7280=ADVANCED_FACE('',(#1169),#7087,.F.);
#7281=ADVANCED_FACE('',(#1170,#708),#901,.T.);
#7282=ADVANCED_FACE('',(#1171,#709),#902,.T.);
#7283=ADVANCED_FACE('',(#1172),#903,.T.);
#7284=ADVANCED_FACE('',(#1173,#710,#711),#904,.T.);
#7285=ADVANCED_FACE('',(#1174),#905,.T.);
#7286=ADVANCED_FACE('',(#1175,#712,#713,#714,#715,#716),#906,.T.);
#7287=ADVANCED_FACE('',(#1176),#7088,.F.);
#7288=ADVANCED_FACE('',(#1177),#7089,.T.);
#7289=ADVANCED_FACE('',(#1178,#717,#718,#719,#720,#721),#907,.F.);
#7290=ADVANCED_FACE('',(#1179),#7090,.F.);
#7291=ADVANCED_FACE('',(#1180),#7091,.F.);
#7292=ADVANCED_FACE('',(#1181),#7092,.F.);
#7293=ADVANCED_FACE('',(#1182),#7093,.F.);
#7294=ADVANCED_FACE('',(#1183),#7094,.T.);
#7295=ADVANCED_FACE('',(#1184,#722),#908,.T.);
#7296=ADVANCED_FACE('',(#1185),#7095,.F.);
#7297=ADVANCED_FACE('',(#1186),#7096,.T.);
#7298=ADVANCED_FACE('',(#1187,#723,#724,#725,#726,#727),#909,.T.);
#7299=ADVANCED_FACE('',(#1188,#728,#729,#730,#731,#732),#910,.F.);
#7300=ADVANCED_FACE('',(#1189),#7097,.F.);
#7301=ADVANCED_FACE('',(#1190),#7098,.F.);
#7302=ADVANCED_FACE('',(#1191),#7099,.F.);
#7303=ADVANCED_FACE('',(#1192),#7100,.F.);
#7304=ADVANCED_FACE('',(#1193),#7101,.T.);
#7305=ADVANCED_FACE('',(#1194,#733),#911,.F.);
#7306=ADVANCED_FACE('',(#1195),#7102,.F.);
#7307=ADVANCED_FACE('',(#1196),#7103,.T.);
#7308=ADVANCED_FACE('',(#1197,#734,#735,#736,#737,#738),#912,.T.);
#7309=ADVANCED_FACE('',(#1198,#739,#740,#741,#742,#743),#913,.F.);
#7310=ADVANCED_FACE('',(#1199),#7104,.F.);
#7311=ADVANCED_FACE('',(#1200),#7105,.F.);
#7312=ADVANCED_FACE('',(#1201),#7106,.F.);
#7313=ADVANCED_FACE('',(#1202),#7107,.F.);
#7314=ADVANCED_FACE('',(#1203),#914,.T.);
#7315=ADVANCED_FACE('',(#1204),#915,.T.);
#7316=ADVANCED_FACE('',(#1205),#916,.F.);
#7317=ADVANCED_FACE('',(#1206),#917,.T.);
#7318=ADVANCED_FACE('',(#1207),#918,.T.);
#7319=ADVANCED_FACE('',(#1208),#7108,.F.);
#7320=ADVANCED_FACE('',(#1209,#744),#7109,.T.);
#7321=ADVANCED_FACE('',(#1210,#745,#746,#747,#748,#749),#919,.T.);
#7322=ADVANCED_FACE('',(#1211,#750,#751,#752,#753,#754),#920,.F.);
#7323=ADVANCED_FACE('',(#1212),#7110,.F.);
#7324=ADVANCED_FACE('',(#1213),#7111,.F.);
#7325=ADVANCED_FACE('',(#1214),#7112,.F.);
#7326=ADVANCED_FACE('',(#1215),#7113,.F.);
#7327=ADVANCED_FACE('',(#1216),#7114,.T.);
#7328=ADVANCED_FACE('',(#1217,#755),#921,.T.);
#7329=ADVANCED_FACE('',(#1218),#7115,.F.);
#7330=ADVANCED_FACE('',(#1219),#7116,.T.);
#7331=ADVANCED_FACE('',(#1220,#756,#757,#758,#759,#760),#922,.T.);
#7332=ADVANCED_FACE('',(#1221,#761,#762,#763,#764,#765),#923,.F.);
#7333=ADVANCED_FACE('',(#1222),#7117,.F.);
#7334=ADVANCED_FACE('',(#1223),#7118,.F.);
#7335=ADVANCED_FACE('',(#1224),#7119,.F.);
#7336=ADVANCED_FACE('',(#1225),#7120,.F.);
#7337=ADVANCED_FACE('',(#1226),#7121,.T.);
#7338=ADVANCED_FACE('',(#1227,#766),#924,.F.);
#7339=ADVANCED_FACE('',(#1228),#7122,.F.);
#7340=ADVANCED_FACE('',(#1229),#7123,.T.);
#7341=ADVANCED_FACE('',(#1230,#767,#768,#769,#770,#771),#925,.T.);
#7342=ADVANCED_FACE('',(#1231,#772,#773,#774,#775,#776),#926,.F.);
#7343=ADVANCED_FACE('',(#1232),#7124,.F.);
#7344=ADVANCED_FACE('',(#1233),#927,.T.);
#7345=ADVANCED_FACE('',(#1234),#7125,.F.);
#7346=ADVANCED_FACE('',(#1235),#928,.T.);
#7347=ADVANCED_FACE('',(#1236),#7126,.F.);
#7348=ADVANCED_FACE('',(#1237,#777),#929,.T.);
#7349=ADVANCED_FACE('',(#1238),#7127,.F.);
#7350=ADVANCED_FACE('',(#1239,#778),#930,.T.);
#7351=ADVANCED_FACE('',(#1240),#7128,.F.);
#7352=ADVANCED_FACE('',(#1241,#779),#931,.T.);
#7353=ADVANCED_FACE('',(#1242),#7129,.F.);
#7354=ADVANCED_FACE('',(#1243,#780),#932,.T.);
#7355=ADVANCED_FACE('',(#1244),#7130,.F.);
#7356=ADVANCED_FACE('',(#1245),#7131,.F.);
#7357=ADVANCED_FACE('',(#1246),#7132,.F.);
#7358=ADVANCED_FACE('',(#1247),#7133,.F.);
#7359=ADVANCED_FACE('',(#1248),#933,.T.);
#7360=ADVANCED_FACE('',(#1249),#934,.T.);
#7361=ADVANCED_FACE('',(#1250),#935,.T.);
#7362=ADVANCED_FACE('',(#1251),#936,.T.);
#7363=ADVANCED_FACE('',(#1252,#781,#782,#783,#784,#785,#786),#937,.T.);
#7364=ADVANCED_FACE('',(#1253,#787,#788,#789,#790),#938,.F.);
#7365=ADVANCED_FACE('',(#1254),#7134,.F.);
#7366=ADVANCED_FACE('',(#1255),#7135,.F.);
#7367=ADVANCED_FACE('',(#1256,#791),#939,.T.);
#7368=ADVANCED_FACE('',(#1257),#940,.T.);
#7369=ADVANCED_FACE('',(#1258),#941,.T.);
#7370=ADVANCED_FACE('',(#1259,#792),#942,.T.);
#7371=ADVANCED_FACE('',(#1260),#943,.F.);
#7372=ADVANCED_FACE('',(#1261),#944,.T.);
#7373=ADVANCED_FACE('',(#1262),#945,.T.);
#7374=ADVANCED_FACE('',(#1263),#946,.T.);
#7375=ADVANCED_FACE('',(#1264),#947,.T.);
#7376=ADVANCED_FACE('',(#1265,#793,#794),#948,.F.);
#7377=ADVANCED_FACE('',(#1266),#7136,.F.);
#7378=ADVANCED_FACE('',(#1267,#795),#949,.T.);
#7379=ADVANCED_FACE('',(#1268),#7137,.F.);
#7380=ADVANCED_FACE('',(#1269,#796),#950,.T.);
#7381=ADVANCED_FACE('',(#1270),#7138,.T.);
#7382=ADVANCED_FACE('',(#1271),#951,.T.);
#7383=ADVANCED_FACE('',(#1272),#952,.T.);
#7384=ADVANCED_FACE('',(#1273),#7139,.F.);
#7385=ADVANCED_FACE('',(#1274,#797),#953,.T.);
#7386=ADVANCED_FACE('',(#1275),#7140,.F.);
#7387=ADVANCED_FACE('',(#1276,#798),#954,.T.);
#7388=ADVANCED_FACE('',(#1277),#7141,.T.);
#7389=ADVANCED_FACE('',(#1278),#955,.T.);
#7390=ADVANCED_FACE('',(#1279),#956,.T.);
#7391=ADVANCED_FACE('',(#1280),#7142,.F.);
#7392=ADVANCED_FACE('',(#1281,#799),#957,.T.);
#7393=ADVANCED_FACE('',(#1282),#7143,.F.);
#7394=ADVANCED_FACE('',(#1283,#800),#958,.T.);
#7395=ADVANCED_FACE('',(#1284),#7144,.T.);
#7396=ADVANCED_FACE('',(#1285),#959,.F.);
#7397=ADVANCED_FACE('',(#1286),#960,.T.);
#7398=ADVANCED_FACE('',(#1287),#7145,.F.);
#7399=ADVANCED_FACE('',(#1288,#801),#961,.T.);
#7400=ADVANCED_FACE('',(#1289),#7146,.F.);
#7401=ADVANCED_FACE('',(#1290,#802),#962,.T.);
#7402=ADVANCED_FACE('',(#1291),#7147,.T.);
#7403=ADVANCED_FACE('',(#1292),#963,.T.);
#7404=ADVANCED_FACE('',(#1293),#964,.T.);
#7405=ADVANCED_FACE('',(#1294),#965,.F.);
#7406=ADVANCED_FACE('',(#1295),#966,.F.);
#7407=ADVANCED_FACE('',(#1296),#967,.F.);
#7408=ADVANCED_FACE('',(#1297),#968,.F.);
#7409=ADVANCED_FACE('',(#1298),#969,.T.);
#7410=ADVANCED_FACE('',(#1299,#803),#970,.T.);
#7411=ADVANCED_FACE('',(#1300),#971,.F.);
#7412=ADVANCED_FACE('',(#1301,#804),#972,.F.);
#7413=ADVANCED_FACE('',(#1302,#805),#973,.T.);
#7414=ADVANCED_FACE('',(#1303,#806),#974,.T.);
#7415=ADVANCED_FACE('',(#1304),#975,.T.);
#7416=ADVANCED_FACE('',(#1305,#807),#976,.T.);
#7417=ADVANCED_FACE('',(#1306),#977,.T.);
#7418=ADVANCED_FACE('',(#1307,#808,#809,#810,#811,#812),#978,.T.);
#7419=ADVANCED_FACE('',(#1308),#979,.T.);
#7420=ADVANCED_FACE('',(#1309),#980,.T.);
#7421=ADVANCED_FACE('',(#1310),#981,.T.);
#7422=ADVANCED_FACE('',(#1311),#982,.T.);
#7423=ADVANCED_FACE('',(#1312),#983,.T.);
#7424=ADVANCED_FACE('',(#1313),#984,.F.);
#7425=ADVANCED_FACE('',(#1314),#985,.T.);
#7426=ADVANCED_FACE('',(#1315),#986,.T.);
#7427=ADVANCED_FACE('',(#1316),#987,.T.);
#7428=ADVANCED_FACE('',(#1317),#988,.T.);
#7429=ADVANCED_FACE('',(#1318),#989,.T.);
#7430=ADVANCED_FACE('',(#1319),#990,.F.);
#7431=ADVANCED_FACE('',(#1320),#991,.F.);
#7432=ADVANCED_FACE('',(#1321),#992,.F.);
#7433=ADVANCED_FACE('',(#1322),#993,.F.);
#7434=ADVANCED_FACE('',(#1323),#994,.F.);
#7435=ADVANCED_FACE('',(#1324),#995,.F.);
#7436=ADVANCED_FACE('',(#1325),#996,.F.);
#7437=ADVANCED_FACE('',(#1326),#997,.F.);
#7438=ADVANCED_FACE('',(#1327),#998,.F.);
#7439=ADVANCED_FACE('',(#1328),#999,.F.);
#7440=ADVANCED_FACE('',(#1329),#1000,.T.);
#7441=ADVANCED_FACE('',(#1330),#429,.T.);
#7442=ADVANCED_FACE('',(#1331),#7148,.T.);
#7443=ADVANCED_FACE('',(#1332),#430,.T.);
#7444=ADVANCED_FACE('',(#1333,#813),#1001,.T.);
#7445=ADVANCED_FACE('',(#1334),#431,.T.);
#7446=ADVANCED_FACE('',(#1335),#7149,.T.);
#7447=ADVANCED_FACE('',(#1336),#425,.F.);
#7448=ADVANCED_FACE('',(#1337),#7150,.T.);
#7449=ADVANCED_FACE('',(#1338),#7151,.F.);
#7450=ADVANCED_FACE('',(#1339),#432,.F.);
#7451=ADVANCED_FACE('',(#1340,#814),#1002,.T.);
#7452=ADVANCED_FACE('',(#1341),#7152,.T.);
#7453=ADVANCED_FACE('',(#1342,#815),#1003,.T.);
#7454=ADVANCED_FACE('',(#1343),#433,.F.);
#7455=ADVANCED_FACE('',(#1344),#426,.F.);
#7456=ADVANCED_FACE('',(#1345),#7153,.F.);
#7457=ADVANCED_FACE('',(#1346,#816),#1004,.T.);
#7458=ADVANCED_FACE('',(#1347),#434,.T.);
#7459=ADVANCED_FACE('',(#1348),#7154,.T.);
#7460=ADVANCED_FACE('',(#1349),#435,.T.);
#7461=ADVANCED_FACE('',(#1350,#817),#1005,.T.);
#7462=ADVANCED_FACE('',(#1351),#7155,.F.);
#7463=ADVANCED_FACE('',(#1352),#395,.T.);
#7464=ADVANCED_FACE('',(#1353),#396,.T.);
#7465=ADVANCED_FACE('',(#1354),#397,.T.);
#7466=ADVANCED_FACE('',(#1355),#398,.T.);
#7467=ADVANCED_FACE('',(#1356),#399,.T.);
#7468=ADVANCED_FACE('',(#1357),#400,.T.);
#7469=ADVANCED_FACE('',(#1358),#401,.T.);
#7470=ADVANCED_FACE('',(#1359),#402,.F.);
#7471=ADVANCED_FACE('',(#1360),#7156,.T.);
#7472=ADVANCED_FACE('',(#1361),#1006,.T.);
#7473=ADVANCED_FACE('',(#1362),#403,.F.);
#7474=ADVANCED_FACE('',(#1363),#1007,.T.);
#7475=ADVANCED_FACE('',(#1364),#404,.F.);
#7476=ADVANCED_FACE('',(#1365),#1008,.T.);
#7477=ADVANCED_FACE('',(#1366),#405,.F.);
#7478=ADVANCED_FACE('',(#1367),#1009,.T.);
#7479=ADVANCED_FACE('',(#1368),#406,.F.);
#7480=ADVANCED_FACE('',(#1369),#1010,.T.);
#7481=ADVANCED_FACE('',(#1370),#407,.F.);
#7482=ADVANCED_FACE('',(#1371),#7157,.F.);
#7483=ADVANCED_FACE('',(#1372),#1011,.T.);
#7484=ADVANCED_FACE('',(#1373),#408,.F.);
#7485=ADVANCED_FACE('',(#1374,#818),#1012,.T.);
#7486=ADVANCED_FACE('',(#1375),#1013,.T.);
#7487=ADVANCED_FACE('',(#1376,#819),#1014,.T.);
#7488=ADVANCED_FACE('',(#1377),#7158,.T.);
#7489=ADVANCED_FACE('',(#1378,#820),#1015,.T.);
#7490=ADVANCED_FACE('',(#1379),#7159,.F.);
#7491=ADVANCED_FACE('',(#1380,#821),#1016,.T.);
#7492=ADVANCED_FACE('',(#1381),#7160,.T.);
#7493=ADVANCED_FACE('',(#1382,#822),#1017,.T.);
#7494=ADVANCED_FACE('',(#1383),#7161,.F.);
#7495=ADVANCED_FACE('',(#1384),#427,.F.);
#7496=ADVANCED_FACE('',(#1385),#7162,.T.);
#7497=ADVANCED_FACE('',(#1386),#7163,.F.);
#7498=ADVANCED_FACE('',(#1387),#436,.F.);
#7499=ADVANCED_FACE('',(#1388,#823),#1018,.T.);
#7500=ADVANCED_FACE('',(#1389),#7164,.T.);
#7501=ADVANCED_FACE('',(#1390,#824),#1019,.T.);
#7502=ADVANCED_FACE('',(#1391),#437,.F.);
#7503=ADVANCED_FACE('',(#1392),#428,.F.);
#7504=ADVANCED_FACE('',(#1393),#7165,.F.);
#7505=ADVANCED_FACE('',(#1394,#825),#1020,.T.);
#7506=ADVANCED_FACE('',(#1395),#438,.T.);
#7507=ADVANCED_FACE('',(#1396),#7166,.T.);
#7508=ADVANCED_FACE('',(#1397),#439,.T.);
#7509=ADVANCED_FACE('',(#1398,#826),#1021,.T.);
#7510=ADVANCED_FACE('',(#1399),#7167,.F.);
#7511=ADVANCED_FACE('',(#1400),#409,.T.);
#7512=ADVANCED_FACE('',(#1401),#410,.T.);
#7513=ADVANCED_FACE('',(#1402),#411,.T.);
#7514=ADVANCED_FACE('',(#1403),#412,.T.);
#7515=ADVANCED_FACE('',(#1404),#413,.T.);
#7516=ADVANCED_FACE('',(#1405),#414,.T.);
#7517=ADVANCED_FACE('',(#1406),#415,.T.);
#7518=ADVANCED_FACE('',(#1407),#416,.T.);
#7519=ADVANCED_FACE('',(#1408),#417,.F.);
#7520=ADVANCED_FACE('',(#1409),#7168,.T.);
#7521=ADVANCED_FACE('',(#1410),#1022,.T.);
#7522=ADVANCED_FACE('',(#1411),#418,.F.);
#7523=ADVANCED_FACE('',(#1412),#1023,.T.);
#7524=ADVANCED_FACE('',(#1413),#419,.F.);
#7525=ADVANCED_FACE('',(#1414),#1024,.T.);
#7526=ADVANCED_FACE('',(#1415),#420,.F.);
#7527=ADVANCED_FACE('',(#1416),#1025,.T.);
#7528=ADVANCED_FACE('',(#1417),#421,.F.);
#7529=ADVANCED_FACE('',(#1418),#1026,.T.);
#7530=ADVANCED_FACE('',(#1419),#422,.F.);
#7531=ADVANCED_FACE('',(#1420),#1027,.T.);
#7532=ADVANCED_FACE('',(#1421),#423,.F.);
#7533=ADVANCED_FACE('',(#1422),#7169,.F.);
#7534=ADVANCED_FACE('',(#1423),#1028,.T.);
#7535=ADVANCED_FACE('',(#1424),#424,.F.);
#7536=ADVANCED_FACE('',(#1425,#827),#1029,.T.);
#7537=ADVANCED_FACE('',(#1426),#1030,.T.);
#7538=ADVANCED_FACE('',(#1427,#828),#1031,.T.);
#7539=ADVANCED_FACE('',(#1428),#7170,.T.);
#7540=ADVANCED_FACE('',(#1429,#829),#1032,.T.);
#7541=ADVANCED_FACE('',(#1430),#7171,.F.);
#7542=ADVANCED_FACE('',(#1431,#830),#1033,.T.);
#7543=ADVANCED_FACE('',(#1432),#7172,.T.);
#7544=ADVANCED_FACE('',(#1433,#831),#1034,.T.);
#7545=ADVANCED_FACE('',(#1434),#7173,.F.);
#7546=ADVANCED_FACE('',(#1435),#1035,.T.);
#7547=ADVANCED_FACE('',(#1436),#440,.T.);
#7548=ADVANCED_FACE('',(#1437),#7174,.T.);
#7549=ADVANCED_FACE('',(#1438),#441,.T.);
#7550=ADVANCED_FACE('',(#1439,#832),#1036,.T.);
#7551=ADVANCED_FACE('',(#1440),#442,.T.);
#7552=ADVANCED_FACE('',(#1441),#7175,.T.);
#7553=ADVANCED_FACE('',(#1442),#443,.T.);
#7554=ADVANCED_FACE('',(#1443),#1037,.T.);
#7555=ADVANCED_FACE('',(#1444),#1038,.F.);
#7556=ADVANCED_FACE('',(#1445),#1039,.F.);
#7557=ADVANCED_FACE('',(#1446),#1040,.F.);
#7558=ADVANCED_FACE('',(#1447),#1041,.F.);
#7559=ADVANCED_FACE('',(#1448),#1042,.F.);
#7560=ADVANCED_FACE('',(#1449),#1043,.F.);
#7561=ADVANCED_FACE('',(#1450),#1044,.F.);
#7562=ADVANCED_FACE('',(#1451),#1045,.F.);
#7563=ADVANCED_FACE('',(#1452),#1046,.F.);
#7564=ADVANCED_FACE('',(#1453),#1047,.F.);
#7565=ADVANCED_FACE('',(#1454),#1048,.F.);
#7566=ADVANCED_FACE('',(#1455),#1049,.F.);
#7567=ADVANCED_FACE('',(#1456),#1050,.F.);
#7568=ADVANCED_FACE('',(#1457),#1051,.F.);
#7569=ADVANCED_FACE('',(#1458),#1052,.F.);
#7570=ADVANCED_FACE('',(#1459),#1053,.F.);
#7571=ADVANCED_FACE('',(#1460),#1054,.F.);
#7572=ADVANCED_FACE('',(#1461),#1055,.T.);
#7573=ADVANCED_FACE('',(#1462),#444,.T.);
#7574=ADVANCED_FACE('',(#1463),#7176,.T.);
#7575=ADVANCED_FACE('',(#1464),#445,.T.);
#7576=ADVANCED_FACE('',(#1465,#833),#1056,.T.);
#7577=ADVANCED_FACE('',(#1466),#446,.T.);
#7578=ADVANCED_FACE('',(#1467),#7177,.T.);
#7579=ADVANCED_FACE('',(#1468),#7178,.T.);
#7580=ADVANCED_FACE('',(#1469),#1057,.T.);
#7581=ADVANCED_FACE('',(#1470),#7179,.T.);
#7582=ADVANCED_FACE('',(#1471),#1058,.F.);
#7583=ADVANCED_FACE('',(#1472),#7180,.T.);
#7584=ADVANCED_FACE('',(#1473,#834),#1059,.T.);
#7585=ADVANCED_FACE('',(#1474,#835),#1060,.F.);
#7586=ADVANCED_FACE('',(#1475),#7181,.F.);
#7587=ADVANCED_FACE('',(#1476),#7182,.T.);
#7588=ADVANCED_FACE('',(#1477,#836),#1061,.T.);
#7589=ADVANCED_FACE('',(#1478,#837),#1062,.F.);
#7590=ADVANCED_FACE('',(#1479),#7183,.F.);
#7591=ADVANCED_FACE('',(#1480),#7184,.T.);
#7592=ADVANCED_FACE('',(#1481,#838),#1063,.T.);
#7593=ADVANCED_FACE('',(#1482,#839),#1064,.F.);
#7594=ADVANCED_FACE('',(#1483),#1065,.T.);
#7595=ADVANCED_FACE('',(#1484),#7185,.F.);
#7596=ADVANCED_FACE('',(#1485),#1066,.T.);
#7597=ADVANCED_FACE('',(#1486,#840),#7186,.F.);
#7598=ADVANCED_FACE('',(#1487,#841),#7187,.T.);
#7599=ADVANCED_FACE('',(#1488,#842),#1067,.T.);
#7600=ADVANCED_FACE('',(#1489,#843),#1068,.F.);
#7601=ADVANCED_FACE('',(#1490),#1069,.T.);
#7602=ADVANCED_FACE('',(#1491),#7188,.F.);
#7603=ADVANCED_FACE('',(#1492),#1070,.T.);
#7604=ADVANCED_FACE('',(#1493,#844),#7189,.F.);
#7605=ADVANCED_FACE('',(#1494,#845),#7190,.T.);
#7606=ADVANCED_FACE('',(#1495,#846),#1071,.T.);
#7607=ADVANCED_FACE('',(#1496,#847),#1072,.F.);
#7608=ADVANCED_FACE('',(#1497),#7191,.F.);
#7609=ADVANCED_FACE('',(#1498),#7192,.T.);
#7610=ADVANCED_FACE('',(#1499,#848),#1073,.T.);
#7611=ADVANCED_FACE('',(#1500,#849),#1074,.F.);
#7612=ADVANCED_FACE('',(#1501),#7193,.F.);
#7613=ADVANCED_FACE('',(#1502),#7194,.T.);
#7614=ADVANCED_FACE('',(#1503,#850),#1075,.T.);
#7615=ADVANCED_FACE('',(#1504,#851),#1076,.F.);
#7616=ADVANCED_FACE('',(#1505),#1077,.T.);
#7617=ADVANCED_FACE('',(#1506),#7195,.F.);
#7618=ADVANCED_FACE('',(#1507),#1078,.T.);
#7619=ADVANCED_FACE('',(#1508,#852),#7196,.F.);
#7620=ADVANCED_FACE('',(#1509,#853),#7197,.T.);
#7621=ADVANCED_FACE('',(#1510,#854),#1079,.T.);
#7622=ADVANCED_FACE('',(#1511,#855),#1080,.F.);
#7623=ADVANCED_FACE('',(#1512),#1081,.T.);
#7624=ADVANCED_FACE('',(#1513),#7198,.F.);
#7625=ADVANCED_FACE('',(#1514),#1082,.T.);
#7626=ADVANCED_FACE('',(#1515,#856),#7199,.F.);
#7627=ADVANCED_FACE('',(#1516,#857),#7200,.T.);
#7628=ADVANCED_FACE('',(#1517,#858),#1083,.T.);
#7629=ADVANCED_FACE('',(#1518,#859),#1084,.F.);
#7630=ADVANCED_FACE('',(#1519),#1085,.T.);
#7631=ADVANCED_FACE('',(#1520),#7201,.F.);
#7632=ADVANCED_FACE('',(#1521),#1086,.T.);
#7633=ADVANCED_FACE('',(#1522),#7202,.F.);
#7634=ADVANCED_FACE('',(#1523),#7203,.F.);
#7635=ADVANCED_FACE('',(#1524),#7204,.F.);
#7636=ADVANCED_FACE('',(#1525),#7205,.F.);
#7637=ADVANCED_FACE('',(#1526,#860,#861,#862,#863,#864),#1087,.T.);
#7638=ADVANCED_FACE('',(#1527),#7206,.T.);
#7639=ADVANCED_FACE('',(#1528,#865),#7207,.F.);
#7640=ADVANCED_FACE('',(#1529,#866),#7208,.T.);
#7641=ADVANCED_FACE('',(#1530,#867),#1088,.T.);
#7642=ADVANCED_FACE('',(#1531,#868,#869,#870,#871,#872),#1089,.F.);
#7643=ADVANCED_FACE('',(#1532),#1090,.F.);
#7644=ADVANCED_FACE('',(#1533),#1091,.F.);
#7645=ADVANCED_FACE('',(#1534),#1092,.F.);
#7646=ADVANCED_FACE('',(#1535),#1093,.F.);
#7647=ADVANCED_FACE('',(#1536),#1094,.F.);
#7648=ADVANCED_FACE('',(#1537),#1095,.F.);
#7649=ADVANCED_FACE('',(#1538),#1096,.F.);
#7650=ADVANCED_FACE('',(#1539,#873),#1097,.T.);
#7651=ADVANCED_FACE('',(#1540),#447,.T.);
#7652=ADVANCED_FACE('',(#1541),#7209,.T.);
#7653=ADVANCED_FACE('',(#1542),#448,.T.);
#7654=ADVANCED_FACE('',(#1543),#1098,.T.);
#7655=CLOSED_SHELL('',(#7210,#7211,#7212,#7213,#7214,#7215,#7216,#7217,
#7218,#7219,#7220,#7221,#7222,#7223,#7224,#7225,#7226,#7227));
#7656=CLOSED_SHELL('',(#7228,#7229,#7230,#7231,#7232,#7233,#7234,#7235,
#7236,#7237,#7238,#7239,#7240,#7241,#7242,#7243,#7244,#7245,#7246,#7247,
#7248));
#7657=CLOSED_SHELL('',(#7249,#7250,#7251,#7252,#7253,#7254,#7255,#7256,
#7257,#7258));
#7658=CLOSED_SHELL('',(#7259,#7260,#7261,#7262,#7263,#7264,#7265,#7266,
#7267,#7268));
#7659=CLOSED_SHELL('',(#7269,#7270,#7271,#7272,#7273,#7274,#7275,#7276,
#7277,#7278,#7279,#7280,#7281,#7282,#7283,#7284,#7285,#7286,#7287,#7288,
#7289));
#7660=CLOSED_SHELL('',(#7290,#7291,#7292,#7293,#7294,#7295,#7296,#7297,
#7298,#7299));
#7661=CLOSED_SHELL('',(#7300,#7301,#7302,#7303,#7304,#7305,#7306,#7307,
#7308,#7309));
#7662=CLOSED_SHELL('',(#7310,#7311,#7312,#7313,#7314,#7315,#7316,#7317,
#7318,#7319,#7320,#7321,#7322));
#7663=CLOSED_SHELL('',(#7323,#7324,#7325,#7326,#7327,#7328,#7329,#7330,
#7331,#7332));
#7664=CLOSED_SHELL('',(#7333,#7334,#7335,#7336,#7337,#7338,#7339,#7340,
#7341,#7342));
#7665=CLOSED_SHELL('',(#7343,#7344,#7345,#7346,#7347,#7348,#7349,#7350,
#7351,#7352,#7353,#7354,#7355,#7356,#7357,#7358,#7359,#7360,#7361,#7362,
#7363,#7364));
#7666=CLOSED_SHELL('',(#7365,#7366,#7367,#7368,#7369,#7370,#7371,#7372,
#7373,#7374,#7375,#7376));
#7667=CLOSED_SHELL('',(#7377,#7378,#7379,#7380,#7381,#7382,#7383,#7384,
#7385,#7386,#7387,#7388,#7389,#7390,#7391,#7392,#7393,#7394,#7395,#7396,
#7397,#7398,#7399,#7400,#7401,#7402,#7403,#7404,#7405,#7406,#7407,#7408,
#7409,#7410,#7411,#7412,#7413,#7414,#7415,#7416,#7417,#7418));
#7668=CLOSED_SHELL('',(#7419,#7420,#7421,#7422,#7423,#7424));
#7669=CLOSED_SHELL('',(#7425,#7426,#7427,#7428,#7429,#7430));
#7670=CLOSED_SHELL('',(#7431,#7432,#7433,#7434,#7435,#7436,#7437,#7438));
#7671=CLOSED_SHELL('',(#7439,#7440,#7441,#7442,#7443,#7444,#7445,#7446));
#7672=CLOSED_SHELL('',(#7447,#7448,#7449,#7450,#7451,#7452,#7453,#7454));
#7673=CLOSED_SHELL('',(#7455,#7456,#7457,#7458,#7459,#7460,#7461,#7462));
#7674=CLOSED_SHELL('',(#7463));
#7675=CLOSED_SHELL('',(#7464));
#7676=CLOSED_SHELL('',(#7465));
#7677=CLOSED_SHELL('',(#7466));
#7678=CLOSED_SHELL('',(#7467));
#7679=CLOSED_SHELL('',(#7468));
#7680=CLOSED_SHELL('',(#7469));
#7681=CLOSED_SHELL('',(#7470,#7471,#7472,#7473,#7474,#7475,#7476,#7477,
#7478,#7479,#7480,#7481,#7482,#7483,#7484,#7485,#7486));
#7682=CLOSED_SHELL('',(#7487,#7488,#7489,#7490));
#7683=CLOSED_SHELL('',(#7491,#7492,#7493,#7494));
#7684=CLOSED_SHELL('',(#7495,#7496,#7497,#7498,#7499,#7500,#7501,#7502));
#7685=CLOSED_SHELL('',(#7503,#7504,#7505,#7506,#7507,#7508,#7509,#7510));
#7686=CLOSED_SHELL('',(#7511));
#7687=CLOSED_SHELL('',(#7512));
#7688=CLOSED_SHELL('',(#7513));
#7689=CLOSED_SHELL('',(#7514));
#7690=CLOSED_SHELL('',(#7515));
#7691=CLOSED_SHELL('',(#7516));
#7692=CLOSED_SHELL('',(#7517));
#7693=CLOSED_SHELL('',(#7518));
#7694=CLOSED_SHELL('',(#7519,#7520,#7521,#7522,#7523,#7524,#7525,#7526,
#7527,#7528,#7529,#7530,#7531,#7532,#7533,#7534,#7535,#7536,#7537));
#7695=CLOSED_SHELL('',(#7538,#7539,#7540,#7541));
#7696=CLOSED_SHELL('',(#7542,#7543,#7544,#7545));
#7697=CLOSED_SHELL('',(#7546,#7547,#7548,#7549,#7550,#7551,#7552,#7553,
#7554));
#7698=CLOSED_SHELL('',(#7555,#7556,#7557,#7558,#7559,#7560,#7561,#7562));
#7699=CLOSED_SHELL('',(#7563,#7564,#7565,#7566,#7567,#7568,#7569,#7570));
#7700=CLOSED_SHELL('',(#7571,#7572,#7573,#7574,#7575,#7576,#7577,#7578));
#7701=CLOSED_SHELL('',(#7579,#7580,#7581,#7582,#7583,#7584,#7585));
#7702=CLOSED_SHELL('',(#7586,#7587,#7588,#7589));
#7703=CLOSED_SHELL('',(#7590,#7591,#7592,#7593));
#7704=CLOSED_SHELL('',(#7594,#7595,#7596,#7597,#7598,#7599,#7600));
#7705=CLOSED_SHELL('',(#7601,#7602,#7603,#7604,#7605,#7606,#7607));
#7706=CLOSED_SHELL('',(#7608,#7609,#7610,#7611));
#7707=CLOSED_SHELL('',(#7612,#7613,#7614,#7615));
#7708=CLOSED_SHELL('',(#7616,#7617,#7618,#7619,#7620,#7621,#7622));
#7709=CLOSED_SHELL('',(#7623,#7624,#7625,#7626,#7627,#7628,#7629));
#7710=CLOSED_SHELL('',(#7630,#7631,#7632,#7633,#7634,#7635,#7636,#7637,
#7638,#7639,#7640,#7641,#7642));
#7711=CLOSED_SHELL('',(#7643,#7644,#7645,#7646,#7647,#7648,#7649,#7650,
#7651,#7652,#7653,#7654));
#7712=DERIVED_UNIT_ELEMENT(#7790,1.);
#7713=DERIVED_UNIT_ELEMENT(#14824,-3.);
#7714=DERIVED_UNIT_ELEMENT(#7790,1.);
#7715=DERIVED_UNIT_ELEMENT(#14824,-3.);
#7716=DERIVED_UNIT_ELEMENT(#7790,1.);
#7717=DERIVED_UNIT_ELEMENT(#14824,-3.);
#7718=DERIVED_UNIT_ELEMENT(#7790,1.);
#7719=DERIVED_UNIT_ELEMENT(#14824,-3.);
#7720=DERIVED_UNIT_ELEMENT(#7790,1.);
#7721=DERIVED_UNIT_ELEMENT(#14824,-3.);
#7722=DERIVED_UNIT_ELEMENT(#7790,1.);
#7723=DERIVED_UNIT_ELEMENT(#14824,-3.);
#7724=DERIVED_UNIT_ELEMENT(#7790,1.);
#7725=DERIVED_UNIT_ELEMENT(#14824,-3.);
#7726=DERIVED_UNIT_ELEMENT(#7790,1.);
#7727=DERIVED_UNIT_ELEMENT(#14824,-3.);
#7728=DERIVED_UNIT_ELEMENT(#7790,1.);
#7729=DERIVED_UNIT_ELEMENT(#14824,-3.);
#7730=DERIVED_UNIT_ELEMENT(#7790,1.);
#7731=DERIVED_UNIT_ELEMENT(#14824,-3.);
#7732=DERIVED_UNIT_ELEMENT(#7790,1.);
#7733=DERIVED_UNIT_ELEMENT(#14824,-3.);
#7734=DERIVED_UNIT_ELEMENT(#7790,1.);
#7735=DERIVED_UNIT_ELEMENT(#14824,-3.);
#7736=DERIVED_UNIT_ELEMENT(#7790,1.);
#7737=DERIVED_UNIT_ELEMENT(#14824,-3.);
#7738=DERIVED_UNIT_ELEMENT(#7790,1.);
#7739=DERIVED_UNIT_ELEMENT(#14824,-3.);
#7740=DERIVED_UNIT_ELEMENT(#7790,1.);
#7741=DERIVED_UNIT_ELEMENT(#14824,-3.);
#7742=DERIVED_UNIT_ELEMENT(#7790,1.);
#7743=DERIVED_UNIT_ELEMENT(#14824,-3.);
#7744=DERIVED_UNIT_ELEMENT(#7790,1.);
#7745=DERIVED_UNIT_ELEMENT(#14824,-3.);
#7746=DERIVED_UNIT_ELEMENT(#7790,1.);
#7747=DERIVED_UNIT_ELEMENT(#14824,-3.);
#7748=DERIVED_UNIT_ELEMENT(#7790,1.);
#7749=DERIVED_UNIT_ELEMENT(#14824,-3.);
#7750=DERIVED_UNIT_ELEMENT(#7790,1.);
#7751=DERIVED_UNIT_ELEMENT(#14824,-3.);
#7752=DERIVED_UNIT_ELEMENT(#7790,1.);
#7753=DERIVED_UNIT_ELEMENT(#14824,-3.);
#7754=DERIVED_UNIT_ELEMENT(#7790,1.);
#7755=DERIVED_UNIT_ELEMENT(#14824,-3.);
#7756=DERIVED_UNIT_ELEMENT(#7790,1.);
#7757=DERIVED_UNIT_ELEMENT(#14824,-3.);
#7758=DERIVED_UNIT_ELEMENT(#7790,1.);
#7759=DERIVED_UNIT_ELEMENT(#14824,-3.);
#7760=DERIVED_UNIT_ELEMENT(#7790,1.);
#7761=DERIVED_UNIT_ELEMENT(#14824,-3.);
#7762=DERIVED_UNIT_ELEMENT(#7790,1.);
#7763=DERIVED_UNIT_ELEMENT(#14824,-3.);
#7764=DERIVED_UNIT_ELEMENT(#7790,1.);
#7765=DERIVED_UNIT_ELEMENT(#14824,-3.);
#7766=DERIVED_UNIT_ELEMENT(#7790,1.);
#7767=DERIVED_UNIT_ELEMENT(#14824,-3.);
#7768=DERIVED_UNIT_ELEMENT(#7790,1.);
#7769=DERIVED_UNIT_ELEMENT(#14824,-3.);
#7770=DERIVED_UNIT_ELEMENT(#7790,1.);
#7771=DERIVED_UNIT_ELEMENT(#14824,-3.);
#7772=DERIVED_UNIT_ELEMENT(#7790,1.);
#7773=DERIVED_UNIT_ELEMENT(#14824,-3.);
#7774=DERIVED_UNIT_ELEMENT(#7790,1.);
#7775=DERIVED_UNIT_ELEMENT(#14824,-3.);
#7776=DERIVED_UNIT_ELEMENT(#7790,1.);
#7777=DERIVED_UNIT_ELEMENT(#14824,-3.);
#7778=DERIVED_UNIT_ELEMENT(#7790,1.);
#7779=DERIVED_UNIT_ELEMENT(#14824,-3.);
#7780=DERIVED_UNIT_ELEMENT(#7790,1.);
#7781=DERIVED_UNIT_ELEMENT(#14824,-3.);
#7782=DERIVED_UNIT_ELEMENT(#7790,1.);
#7783=DERIVED_UNIT_ELEMENT(#14824,-3.);
#7784=DERIVED_UNIT_ELEMENT(#7790,1.);
#7785=DERIVED_UNIT_ELEMENT(#14824,-3.);
#7786=DERIVED_UNIT_ELEMENT(#7790,1.);
#7787=DERIVED_UNIT_ELEMENT(#14824,-3.);
#7788=DERIVED_UNIT_ELEMENT(#7790,1.);
#7789=DERIVED_UNIT_ELEMENT(#14824,-3.);
#7790=(
MASS_UNIT()
NAMED_UNIT(*)
SI_UNIT(.KILO.,.GRAM.)
);
#7791=DERIVED_UNIT((#7712,#7713));
#7792=DERIVED_UNIT((#7714,#7715));
#7793=DERIVED_UNIT((#7716,#7717));
#7794=DERIVED_UNIT((#7718,#7719));
#7795=DERIVED_UNIT((#7720,#7721));
#7796=DERIVED_UNIT((#7722,#7723));
#7797=DERIVED_UNIT((#7724,#7725));
#7798=DERIVED_UNIT((#7726,#7727));
#7799=DERIVED_UNIT((#7728,#7729));
#7800=DERIVED_UNIT((#7730,#7731));
#7801=DERIVED_UNIT((#7732,#7733));
#7802=DERIVED_UNIT((#7734,#7735));
#7803=DERIVED_UNIT((#7736,#7737));
#7804=DERIVED_UNIT((#7738,#7739));
#7805=DERIVED_UNIT((#7740,#7741));
#7806=DERIVED_UNIT((#7742,#7743));
#7807=DERIVED_UNIT((#7744,#7745));
#7808=DERIVED_UNIT((#7746,#7747));
#7809=DERIVED_UNIT((#7748,#7749));
#7810=DERIVED_UNIT((#7750,#7751));
#7811=DERIVED_UNIT((#7752,#7753));
#7812=DERIVED_UNIT((#7754,#7755));
#7813=DERIVED_UNIT((#7756,#7757));
#7814=DERIVED_UNIT((#7758,#7759));
#7815=DERIVED_UNIT((#7760,#7761));
#7816=DERIVED_UNIT((#7762,#7763));
#7817=DERIVED_UNIT((#7764,#7765));
#7818=DERIVED_UNIT((#7766,#7767));
#7819=DERIVED_UNIT((#7768,#7769));
#7820=DERIVED_UNIT((#7770,#7771));
#7821=DERIVED_UNIT((#7772,#7773));
#7822=DERIVED_UNIT((#7774,#7775));
#7823=DERIVED_UNIT((#7776,#7777));
#7824=DERIVED_UNIT((#7778,#7779));
#7825=DERIVED_UNIT((#7780,#7781));
#7826=DERIVED_UNIT((#7782,#7783));
#7827=DERIVED_UNIT((#7784,#7785));
#7828=DERIVED_UNIT((#7786,#7787));
#7829=DERIVED_UNIT((#7788,#7789));
#7830=MEASURE_REPRESENTATION_ITEM('density measure',
POSITIVE_RATIO_MEASURE(7850.),#7791);
#7831=MEASURE_REPRESENTATION_ITEM('density measure',
POSITIVE_RATIO_MEASURE(7850.),#7792);
#7832=MEASURE_REPRESENTATION_ITEM('density measure',
POSITIVE_RATIO_MEASURE(7850.),#7793);
#7833=MEASURE_REPRESENTATION_ITEM('density measure',
POSITIVE_RATIO_MEASURE(7850.),#7794);
#7834=MEASURE_REPRESENTATION_ITEM('density measure',
POSITIVE_RATIO_MEASURE(7850.),#7795);
#7835=MEASURE_REPRESENTATION_ITEM('density measure',
POSITIVE_RATIO_MEASURE(7850.),#7796);
#7836=MEASURE_REPRESENTATION_ITEM('density measure',
POSITIVE_RATIO_MEASURE(7850.),#7797);
#7837=MEASURE_REPRESENTATION_ITEM('density measure',
POSITIVE_RATIO_MEASURE(7850.),#7798);
#7838=MEASURE_REPRESENTATION_ITEM('density measure',
POSITIVE_RATIO_MEASURE(7850.),#7799);
#7839=MEASURE_REPRESENTATION_ITEM('density measure',
POSITIVE_RATIO_MEASURE(7850.),#7800);
#7840=MEASURE_REPRESENTATION_ITEM('density measure',
POSITIVE_RATIO_MEASURE(7850.),#7801);
#7841=MEASURE_REPRESENTATION_ITEM('density measure',
POSITIVE_RATIO_MEASURE(7850.),#7802);
#7842=MEASURE_REPRESENTATION_ITEM('density measure',
POSITIVE_RATIO_MEASURE(7850.),#7803);
#7843=MEASURE_REPRESENTATION_ITEM('density measure',
POSITIVE_RATIO_MEASURE(7850.),#7804);
#7844=MEASURE_REPRESENTATION_ITEM('density measure',
POSITIVE_RATIO_MEASURE(7850.),#7805);
#7845=MEASURE_REPRESENTATION_ITEM('density measure',
POSITIVE_RATIO_MEASURE(7850.),#7806);
#7846=MEASURE_REPRESENTATION_ITEM('density measure',
POSITIVE_RATIO_MEASURE(7850.),#7807);
#7847=MEASURE_REPRESENTATION_ITEM('density measure',
POSITIVE_RATIO_MEASURE(7850.),#7808);
#7848=MEASURE_REPRESENTATION_ITEM('density measure',
POSITIVE_RATIO_MEASURE(7850.),#7809);
#7849=MEASURE_REPRESENTATION_ITEM('density measure',
POSITIVE_RATIO_MEASURE(7850.),#7810);
#7850=MEASURE_REPRESENTATION_ITEM('density measure',
POSITIVE_RATIO_MEASURE(7850.),#7811);
#7851=MEASURE_REPRESENTATION_ITEM('density measure',
POSITIVE_RATIO_MEASURE(7850.),#7812);
#7852=MEASURE_REPRESENTATION_ITEM('density measure',
POSITIVE_RATIO_MEASURE(7850.),#7813);
#7853=MEASURE_REPRESENTATION_ITEM('density measure',
POSITIVE_RATIO_MEASURE(7850.),#7814);
#7854=MEASURE_REPRESENTATION_ITEM('density measure',
POSITIVE_RATIO_MEASURE(7850.),#7815);
#7855=MEASURE_REPRESENTATION_ITEM('density measure',
POSITIVE_RATIO_MEASURE(7850.),#7816);
#7856=MEASURE_REPRESENTATION_ITEM('density measure',
POSITIVE_RATIO_MEASURE(7850.),#7817);
#7857=MEASURE_REPRESENTATION_ITEM('density measure',
POSITIVE_RATIO_MEASURE(7850.),#7818);
#7858=MEASURE_REPRESENTATION_ITEM('density measure',
POSITIVE_RATIO_MEASURE(7850.),#7819);
#7859=MEASURE_REPRESENTATION_ITEM('density measure',
POSITIVE_RATIO_MEASURE(7850.),#7820);
#7860=MEASURE_REPRESENTATION_ITEM('density measure',
POSITIVE_RATIO_MEASURE(7850.),#7821);
#7861=MEASURE_REPRESENTATION_ITEM('density measure',
POSITIVE_RATIO_MEASURE(7850.),#7822);
#7862=MEASURE_REPRESENTATION_ITEM('density measure',
POSITIVE_RATIO_MEASURE(7850.),#7823);
#7863=MEASURE_REPRESENTATION_ITEM('density measure',
POSITIVE_RATIO_MEASURE(7850.),#7824);
#7864=MEASURE_REPRESENTATION_ITEM('density measure',
POSITIVE_RATIO_MEASURE(7850.),#7825);
#7865=MEASURE_REPRESENTATION_ITEM('density measure',
POSITIVE_RATIO_MEASURE(7850.),#7826);
#7866=MEASURE_REPRESENTATION_ITEM('density measure',
POSITIVE_RATIO_MEASURE(7850.),#7827);
#7867=MEASURE_REPRESENTATION_ITEM('density measure',
POSITIVE_RATIO_MEASURE(7850.),#7828);
#7868=MEASURE_REPRESENTATION_ITEM('density measure',
POSITIVE_RATIO_MEASURE(7850.),#7829);
#7869=PROPERTY_DEFINITION_REPRESENTATION(#8064,#7947);
#7870=PROPERTY_DEFINITION_REPRESENTATION(#8065,#7948);
#7871=PROPERTY_DEFINITION_REPRESENTATION(#8066,#7949);
#7872=PROPERTY_DEFINITION_REPRESENTATION(#8067,#7950);
#7873=PROPERTY_DEFINITION_REPRESENTATION(#8068,#7951);
#7874=PROPERTY_DEFINITION_REPRESENTATION(#8069,#7952);
#7875=PROPERTY_DEFINITION_REPRESENTATION(#8070,#7953);
#7876=PROPERTY_DEFINITION_REPRESENTATION(#8071,#7954);
#7877=PROPERTY_DEFINITION_REPRESENTATION(#8072,#7955);
#7878=PROPERTY_DEFINITION_REPRESENTATION(#8073,#7956);
#7879=PROPERTY_DEFINITION_REPRESENTATION(#8074,#7957);
#7880=PROPERTY_DEFINITION_REPRESENTATION(#8075,#7958);
#7881=PROPERTY_DEFINITION_REPRESENTATION(#8076,#7959);
#7882=PROPERTY_DEFINITION_REPRESENTATION(#8077,#7960);
#7883=PROPERTY_DEFINITION_REPRESENTATION(#8078,#7961);
#7884=PROPERTY_DEFINITION_REPRESENTATION(#8079,#7962);
#7885=PROPERTY_DEFINITION_REPRESENTATION(#8080,#7963);
#7886=PROPERTY_DEFINITION_REPRESENTATION(#8081,#7964);
#7887=PROPERTY_DEFINITION_REPRESENTATION(#8082,#7965);
#7888=PROPERTY_DEFINITION_REPRESENTATION(#8083,#7966);
#7889=PROPERTY_DEFINITION_REPRESENTATION(#8084,#7967);
#7890=PROPERTY_DEFINITION_REPRESENTATION(#8085,#7968);
#7891=PROPERTY_DEFINITION_REPRESENTATION(#8086,#7969);
#7892=PROPERTY_DEFINITION_REPRESENTATION(#8087,#7970);
#7893=PROPERTY_DEFINITION_REPRESENTATION(#8088,#7971);
#7894=PROPERTY_DEFINITION_REPRESENTATION(#8089,#7972);
#7895=PROPERTY_DEFINITION_REPRESENTATION(#8090,#7973);
#7896=PROPERTY_DEFINITION_REPRESENTATION(#8091,#7974);
#7897=PROPERTY_DEFINITION_REPRESENTATION(#8092,#7975);
#7898=PROPERTY_DEFINITION_REPRESENTATION(#8093,#7976);
#7899=PROPERTY_DEFINITION_REPRESENTATION(#8094,#7977);
#7900=PROPERTY_DEFINITION_REPRESENTATION(#8095,#7978);
#7901=PROPERTY_DEFINITION_REPRESENTATION(#8096,#7979);
#7902=PROPERTY_DEFINITION_REPRESENTATION(#8097,#7980);
#7903=PROPERTY_DEFINITION_REPRESENTATION(#8098,#7981);
#7904=PROPERTY_DEFINITION_REPRESENTATION(#8099,#7982);
#7905=PROPERTY_DEFINITION_REPRESENTATION(#8100,#7983);
#7906=PROPERTY_DEFINITION_REPRESENTATION(#8101,#7984);
#7907=PROPERTY_DEFINITION_REPRESENTATION(#8102,#7985);
#7908=PROPERTY_DEFINITION_REPRESENTATION(#8103,#7986);
#7909=PROPERTY_DEFINITION_REPRESENTATION(#8104,#7987);
#7910=PROPERTY_DEFINITION_REPRESENTATION(#8105,#7988);
#7911=PROPERTY_DEFINITION_REPRESENTATION(#8106,#7989);
#7912=PROPERTY_DEFINITION_REPRESENTATION(#8107,#7990);
#7913=PROPERTY_DEFINITION_REPRESENTATION(#8108,#7991);
#7914=PROPERTY_DEFINITION_REPRESENTATION(#8109,#7992);
#7915=PROPERTY_DEFINITION_REPRESENTATION(#8110,#7993);
#7916=PROPERTY_DEFINITION_REPRESENTATION(#8111,#7994);
#7917=PROPERTY_DEFINITION_REPRESENTATION(#8112,#7995);
#7918=PROPERTY_DEFINITION_REPRESENTATION(#8113,#7996);
#7919=PROPERTY_DEFINITION_REPRESENTATION(#8114,#7997);
#7920=PROPERTY_DEFINITION_REPRESENTATION(#8115,#7998);
#7921=PROPERTY_DEFINITION_REPRESENTATION(#8116,#7999);
#7922=PROPERTY_DEFINITION_REPRESENTATION(#8117,#8000);
#7923=PROPERTY_DEFINITION_REPRESENTATION(#8118,#8001);
#7924=PROPERTY_DEFINITION_REPRESENTATION(#8119,#8002);
#7925=PROPERTY_DEFINITION_REPRESENTATION(#8120,#8003);
#7926=PROPERTY_DEFINITION_REPRESENTATION(#8121,#8004);
#7927=PROPERTY_DEFINITION_REPRESENTATION(#8122,#8005);
#7928=PROPERTY_DEFINITION_REPRESENTATION(#8123,#8006);
#7929=PROPERTY_DEFINITION_REPRESENTATION(#8124,#8007);
#7930=PROPERTY_DEFINITION_REPRESENTATION(#8125,#8008);
#7931=PROPERTY_DEFINITION_REPRESENTATION(#8126,#8009);
#7932=PROPERTY_DEFINITION_REPRESENTATION(#8127,#8010);
#7933=PROPERTY_DEFINITION_REPRESENTATION(#8128,#8011);
#7934=PROPERTY_DEFINITION_REPRESENTATION(#8129,#8012);
#7935=PROPERTY_DEFINITION_REPRESENTATION(#8130,#8013);
#7936=PROPERTY_DEFINITION_REPRESENTATION(#8131,#8014);
#7937=PROPERTY_DEFINITION_REPRESENTATION(#8132,#8015);
#7938=PROPERTY_DEFINITION_REPRESENTATION(#8133,#8016);
#7939=PROPERTY_DEFINITION_REPRESENTATION(#8134,#8017);
#7940=PROPERTY_DEFINITION_REPRESENTATION(#8135,#8018);
#7941=PROPERTY_DEFINITION_REPRESENTATION(#8136,#8019);
#7942=PROPERTY_DEFINITION_REPRESENTATION(#8137,#8020);
#7943=PROPERTY_DEFINITION_REPRESENTATION(#8138,#8021);
#7944=PROPERTY_DEFINITION_REPRESENTATION(#8139,#8022);
#7945=PROPERTY_DEFINITION_REPRESENTATION(#8140,#8023);
#7946=PROPERTY_DEFINITION_REPRESENTATION(#8141,#8024);
#7947=REPRESENTATION('material name',(#8025),#14780);
#7948=REPRESENTATION('density',(#7830),#14780);
#7949=REPRESENTATION('material name',(#8026),#14781);
#7950=REPRESENTATION('density',(#7831),#14781);
#7951=REPRESENTATION('material name',(#8027),#14782);
#7952=REPRESENTATION('density',(#7832),#14782);
#7953=REPRESENTATION('material name',(#8028),#14783);
#7954=REPRESENTATION('density',(#7833),#14783);
#7955=REPRESENTATION('material name',(#8029),#14784);
#7956=REPRESENTATION('density',(#7834),#14784);
#7957=REPRESENTATION('material name',(#8030),#14785);
#7958=REPRESENTATION('density',(#7835),#14785);
#7959=REPRESENTATION('material name',(#8031),#14786);
#7960=REPRESENTATION('density',(#7836),#14786);
#7961=REPRESENTATION('material name',(#8032),#14787);
#7962=REPRESENTATION('density',(#7837),#14787);
#7963=REPRESENTATION('material name',(#8033),#14788);
#7964=REPRESENTATION('density',(#7838),#14788);
#7965=REPRESENTATION('material name',(#8034),#14789);
#7966=REPRESENTATION('density',(#7839),#14789);
#7967=REPRESENTATION('material name',(#8035),#14790);
#7968=REPRESENTATION('density',(#7840),#14790);
#7969=REPRESENTATION('material name',(#8036),#14791);
#7970=REPRESENTATION('density',(#7841),#14791);
#7971=REPRESENTATION('material name',(#8037),#14792);
#7972=REPRESENTATION('density',(#7842),#14792);
#7973=REPRESENTATION('material name',(#8038),#14793);
#7974=REPRESENTATION('density',(#7843),#14793);
#7975=REPRESENTATION('material name',(#8039),#14794);
#7976=REPRESENTATION('density',(#7844),#14794);
#7977=REPRESENTATION('material name',(#8040),#14795);
#7978=REPRESENTATION('density',(#7845),#14795);
#7979=REPRESENTATION('material name',(#8041),#14797);
#7980=REPRESENTATION('density',(#7846),#14797);
#7981=REPRESENTATION('material name',(#8042),#14798);
#7982=REPRESENTATION('density',(#7847),#14798);
#7983=REPRESENTATION('material name',(#8043),#14799);
#7984=REPRESENTATION('density',(#7848),#14799);
#7985=REPRESENTATION('material name',(#8044),#14800);
#7986=REPRESENTATION('density',(#7849),#14800);
#7987=REPRESENTATION('material name',(#8045),#14801);
#7988=REPRESENTATION('density',(#7850),#14801);
#7989=REPRESENTATION('material name',(#8046),#14803);
#7990=REPRESENTATION('density',(#7851),#14803);
#7991=REPRESENTATION('material name',(#8047),#14804);
#7992=REPRESENTATION('density',(#7852),#14804);
#7993=REPRESENTATION('material name',(#8048),#14805);
#7994=REPRESENTATION('density',(#7853),#14805);
#7995=REPRESENTATION('material name',(#8049),#14806);
#7996=REPRESENTATION('density',(#7854),#14806);
#7997=REPRESENTATION('material name',(#8050),#14807);
#7998=REPRESENTATION('density',(#7855),#14807);
#7999=REPRESENTATION('material name',(#8051),#14808);
#8000=REPRESENTATION('density',(#7856),#14808);
#8001=REPRESENTATION('material name',(#8052),#14809);
#8002=REPRESENTATION('density',(#7857),#14809);
#8003=REPRESENTATION('material name',(#8053),#14811);
#8004=REPRESENTATION('density',(#7858),#14811);
#8005=REPRESENTATION('material name',(#8054),#14812);
#8006=REPRESENTATION('density',(#7859),#14812);
#8007=REPRESENTATION('material name',(#8055),#14813);
#8008=REPRESENTATION('density',(#7860),#14813);
#8009=REPRESENTATION('material name',(#8056),#14814);
#8010=REPRESENTATION('density',(#7861),#14814);
#8011=REPRESENTATION('material name',(#8057),#14815);
#8012=REPRESENTATION('density',(#7862),#14815);
#8013=REPRESENTATION('material name',(#8058),#14816);
#8014=REPRESENTATION('density',(#7863),#14816);
#8015=REPRESENTATION('material name',(#8059),#14817);
#8016=REPRESENTATION('density',(#7864),#14817);
#8017=REPRESENTATION('material name',(#8060),#14818);
#8018=REPRESENTATION('density',(#7865),#14818);
#8019=REPRESENTATION('material name',(#8061),#14819);
#8020=REPRESENTATION('density',(#7866),#14819);
#8021=REPRESENTATION('material name',(#8062),#14820);
#8022=REPRESENTATION('density',(#7867),#14820);
#8023=REPRESENTATION('material name',(#8063),#14821);
#8024=REPRESENTATION('density',(#7868),#14821);
#8025=DESCRIPTIVE_REPRESENTATION_ITEM('Steel','Steel');
#8026=DESCRIPTIVE_REPRESENTATION_ITEM('Steel','Steel');
#8027=DESCRIPTIVE_REPRESENTATION_ITEM('Steel','Steel');
#8028=DESCRIPTIVE_REPRESENTATION_ITEM('Steel','Steel');
#8029=DESCRIPTIVE_REPRESENTATION_ITEM('Steel','Steel');
#8030=DESCRIPTIVE_REPRESENTATION_ITEM('Steel','Steel');
#8031=DESCRIPTIVE_REPRESENTATION_ITEM('Steel','Steel');
#8032=DESCRIPTIVE_REPRESENTATION_ITEM('Steel','Steel');
#8033=DESCRIPTIVE_REPRESENTATION_ITEM('Steel','Steel');
#8034=DESCRIPTIVE_REPRESENTATION_ITEM('Steel','Steel');
#8035=DESCRIPTIVE_REPRESENTATION_ITEM('Steel','Steel');
#8036=DESCRIPTIVE_REPRESENTATION_ITEM('Steel','Steel');
#8037=DESCRIPTIVE_REPRESENTATION_ITEM('Steel','Steel');
#8038=DESCRIPTIVE_REPRESENTATION_ITEM('Steel','Steel');
#8039=DESCRIPTIVE_REPRESENTATION_ITEM('Steel','Steel');
#8040=DESCRIPTIVE_REPRESENTATION_ITEM('Steel','Steel');
#8041=DESCRIPTIVE_REPRESENTATION_ITEM('Steel','Steel');
#8042=DESCRIPTIVE_REPRESENTATION_ITEM('Steel','Steel');
#8043=DESCRIPTIVE_REPRESENTATION_ITEM('Steel','Steel');
#8044=DESCRIPTIVE_REPRESENTATION_ITEM('Steel','Steel');
#8045=DESCRIPTIVE_REPRESENTATION_ITEM('Steel','Steel');
#8046=DESCRIPTIVE_REPRESENTATION_ITEM('Steel','Steel');
#8047=DESCRIPTIVE_REPRESENTATION_ITEM('Steel','Steel');
#8048=DESCRIPTIVE_REPRESENTATION_ITEM('Steel','Steel');
#8049=DESCRIPTIVE_REPRESENTATION_ITEM('Steel','Steel');
#8050=DESCRIPTIVE_REPRESENTATION_ITEM('Steel','Steel');
#8051=DESCRIPTIVE_REPRESENTATION_ITEM('Steel','Steel');
#8052=DESCRIPTIVE_REPRESENTATION_ITEM('Steel','Steel');
#8053=DESCRIPTIVE_REPRESENTATION_ITEM('Steel','Steel');
#8054=DESCRIPTIVE_REPRESENTATION_ITEM('Steel','Steel');
#8055=DESCRIPTIVE_REPRESENTATION_ITEM('Steel','Steel');
#8056=DESCRIPTIVE_REPRESENTATION_ITEM('Steel','Steel');
#8057=DESCRIPTIVE_REPRESENTATION_ITEM('Steel','Steel');
#8058=DESCRIPTIVE_REPRESENTATION_ITEM('Steel','Steel');
#8059=DESCRIPTIVE_REPRESENTATION_ITEM('Steel','Steel');
#8060=DESCRIPTIVE_REPRESENTATION_ITEM('Steel','Steel');
#8061=DESCRIPTIVE_REPRESENTATION_ITEM('Steel','Steel');
#8062=DESCRIPTIVE_REPRESENTATION_ITEM('Steel','Steel');
#8063=DESCRIPTIVE_REPRESENTATION_ITEM('Steel','Steel');
#8064=PROPERTY_DEFINITION('material property','material name',#15045);
#8065=PROPERTY_DEFINITION('material property','density of part',#15045);
#8066=PROPERTY_DEFINITION('material property','material name',#15046);
#8067=PROPERTY_DEFINITION('material property','density of part',#15046);
#8068=PROPERTY_DEFINITION('material property','material name',#15047);
#8069=PROPERTY_DEFINITION('material property','density of part',#15047);
#8070=PROPERTY_DEFINITION('material property','material name',#15048);
#8071=PROPERTY_DEFINITION('material property','density of part',#15048);
#8072=PROPERTY_DEFINITION('material property','material name',#15049);
#8073=PROPERTY_DEFINITION('material property','density of part',#15049);
#8074=PROPERTY_DEFINITION('material property','material name',#15050);
#8075=PROPERTY_DEFINITION('material property','density of part',#15050);
#8076=PROPERTY_DEFINITION('material property','material name',#15051);
#8077=PROPERTY_DEFINITION('material property','density of part',#15051);
#8078=PROPERTY_DEFINITION('material property','material name',#15052);
#8079=PROPERTY_DEFINITION('material property','density of part',#15052);
#8080=PROPERTY_DEFINITION('material property','material name',#15053);
#8081=PROPERTY_DEFINITION('material property','density of part',#15053);
#8082=PROPERTY_DEFINITION('material property','material name',#15054);
#8083=PROPERTY_DEFINITION('material property','density of part',#15054);
#8084=PROPERTY_DEFINITION('material property','material name',#15055);
#8085=PROPERTY_DEFINITION('material property','density of part',#15055);
#8086=PROPERTY_DEFINITION('material property','material name',#15056);
#8087=PROPERTY_DEFINITION('material property','density of part',#15056);
#8088=PROPERTY_DEFINITION('material property','material name',#15057);
#8089=PROPERTY_DEFINITION('material property','density of part',#15057);
#8090=PROPERTY_DEFINITION('material property','material name',#15058);
#8091=PROPERTY_DEFINITION('material property','density of part',#15058);
#8092=PROPERTY_DEFINITION('material property','material name',#15059);
#8093=PROPERTY_DEFINITION('material property','density of part',#15059);
#8094=PROPERTY_DEFINITION('material property','material name',#15060);
#8095=PROPERTY_DEFINITION('material property','density of part',#15060);
#8096=PROPERTY_DEFINITION('material property','material name',#15062);
#8097=PROPERTY_DEFINITION('material property','density of part',#15062);
#8098=PROPERTY_DEFINITION('material property','material name',#15063);
#8099=PROPERTY_DEFINITION('material property','density of part',#15063);
#8100=PROPERTY_DEFINITION('material property','material name',#15064);
#8101=PROPERTY_DEFINITION('material property','density of part',#15064);
#8102=PROPERTY_DEFINITION('material property','material name',#15065);
#8103=PROPERTY_DEFINITION('material property','density of part',#15065);
#8104=PROPERTY_DEFINITION('material property','material name',#15066);
#8105=PROPERTY_DEFINITION('material property','density of part',#15066);
#8106=PROPERTY_DEFINITION('material property','material name',#15068);
#8107=PROPERTY_DEFINITION('material property','density of part',#15068);
#8108=PROPERTY_DEFINITION('material property','material name',#15069);
#8109=PROPERTY_DEFINITION('material property','density of part',#15069);
#8110=PROPERTY_DEFINITION('material property','material name',#15070);
#8111=PROPERTY_DEFINITION('material property','density of part',#15070);
#8112=PROPERTY_DEFINITION('material property','material name',#15071);
#8113=PROPERTY_DEFINITION('material property','density of part',#15071);
#8114=PROPERTY_DEFINITION('material property','material name',#15072);
#8115=PROPERTY_DEFINITION('material property','density of part',#15072);
#8116=PROPERTY_DEFINITION('material property','material name',#15073);
#8117=PROPERTY_DEFINITION('material property','density of part',#15073);
#8118=PROPERTY_DEFINITION('material property','material name',#15074);
#8119=PROPERTY_DEFINITION('material property','density of part',#15074);
#8120=PROPERTY_DEFINITION('material property','material name',#15076);
#8121=PROPERTY_DEFINITION('material property','density of part',#15076);
#8122=PROPERTY_DEFINITION('material property','material name',#15077);
#8123=PROPERTY_DEFINITION('material property','density of part',#15077);
#8124=PROPERTY_DEFINITION('material property','material name',#15078);
#8125=PROPERTY_DEFINITION('material property','density of part',#15078);
#8126=PROPERTY_DEFINITION('material property','material name',#15079);
#8127=PROPERTY_DEFINITION('material property','density of part',#15079);
#8128=PROPERTY_DEFINITION('material property','material name',#15080);
#8129=PROPERTY_DEFINITION('material property','density of part',#15080);
#8130=PROPERTY_DEFINITION('material property','material name',#15081);
#8131=PROPERTY_DEFINITION('material property','density of part',#15081);
#8132=PROPERTY_DEFINITION('material property','material name',#15082);
#8133=PROPERTY_DEFINITION('material property','density of part',#15082);
#8134=PROPERTY_DEFINITION('material property','material name',#15083);
#8135=PROPERTY_DEFINITION('material property','density of part',#15083);
#8136=PROPERTY_DEFINITION('material property','material name',#15084);
#8137=PROPERTY_DEFINITION('material property','density of part',#15084);
#8138=PROPERTY_DEFINITION('material property','material name',#15085);
#8139=PROPERTY_DEFINITION('material property','density of part',#15085);
#8140=PROPERTY_DEFINITION('material property','material name',#15086);
#8141=PROPERTY_DEFINITION('material property','density of part',#15086);
#8142=AXIS2_PLACEMENT_3D('',#11658,#9166,#9167);
#8143=AXIS2_PLACEMENT_3D('',#11659,#9168,#9169);
#8144=AXIS2_PLACEMENT_3D('',#11660,#9170,#9171);
#8145=AXIS2_PLACEMENT_3D('',#11661,#9172,#9173);
#8146=AXIS2_PLACEMENT_3D('',#11663,#9174,#9175);
#8147=AXIS2_PLACEMENT_3D('',#11666,#9177,#9178);
#8148=AXIS2_PLACEMENT_3D('',#11667,#9179,#9180);
#8149=AXIS2_PLACEMENT_3D('',#11669,#9181,#9182);
#8150=AXIS2_PLACEMENT_3D('',#11672,#9184,#9185);
#8151=AXIS2_PLACEMENT_3D('',#11673,#9186,#9187);
#8152=AXIS2_PLACEMENT_3D('',#11675,#9188,#9189);
#8153=AXIS2_PLACEMENT_3D('',#11678,#9191,#9192);
#8154=AXIS2_PLACEMENT_3D('',#11679,#9193,#9194);
#8155=AXIS2_PLACEMENT_3D('',#11681,#9195,#9196);
#8156=AXIS2_PLACEMENT_3D('',#11684,#9198,#9199);
#8157=AXIS2_PLACEMENT_3D('',#11685,#9200,#9201);
#8158=AXIS2_PLACEMENT_3D('',#11687,#9202,#9203);
#8159=AXIS2_PLACEMENT_3D('',#11690,#9205,#9206);
#8160=AXIS2_PLACEMENT_3D('',#11691,#9207,#9208);
#8161=AXIS2_PLACEMENT_3D('',#11693,#9209,#9210);
#8162=AXIS2_PLACEMENT_3D('',#11696,#9212,#9213);
#8163=AXIS2_PLACEMENT_3D('',#11697,#9214,#9215);
#8164=AXIS2_PLACEMENT_3D('',#11699,#9216,#9217);
#8165=AXIS2_PLACEMENT_3D('',#11702,#9219,#9220);
#8166=AXIS2_PLACEMENT_3D('',#11703,#9221,#9222);
#8167=AXIS2_PLACEMENT_3D('',#11705,#9223,#9224);
#8168=AXIS2_PLACEMENT_3D('',#11708,#9226,#9227);
#8169=AXIS2_PLACEMENT_3D('',#11709,#9228,#9229);
#8170=AXIS2_PLACEMENT_3D('',#11711,#9230,#9231);
#8171=AXIS2_PLACEMENT_3D('',#11714,#9233,#9234);
#8172=AXIS2_PLACEMENT_3D('',#11715,#9235,#9236);
#8173=AXIS2_PLACEMENT_3D('',#11717,#9237,#9238);
#8174=AXIS2_PLACEMENT_3D('',#11720,#9240,#9241);
#8175=AXIS2_PLACEMENT_3D('',#11721,#9242,#9243);
#8176=AXIS2_PLACEMENT_3D('',#11723,#9244,#9245);
#8177=AXIS2_PLACEMENT_3D('',#11726,#9247,#9248);
#8178=AXIS2_PLACEMENT_3D('',#11727,#9249,#9250);
#8179=AXIS2_PLACEMENT_3D('',#11729,#9251,#9252);
#8180=AXIS2_PLACEMENT_3D('',#11732,#9254,#9255);
#8181=AXIS2_PLACEMENT_3D('',#11733,#9256,#9257);
#8182=AXIS2_PLACEMENT_3D('',#11742,#9262,#9263);
#8183=AXIS2_PLACEMENT_3D('',#11748,#9267,#9268);
#8184=AXIS2_PLACEMENT_3D('',#11754,#9272,#9273);
#8185=AXIS2_PLACEMENT_3D('',#11757,#9276,#9277);
#8186=AXIS2_PLACEMENT_3D('',#11758,#9278,#9279);
#8187=AXIS2_PLACEMENT_3D('',#11759,#9280,#9281);
#8188=AXIS2_PLACEMENT_3D('',#11760,#9282,#9283);
#8189=AXIS2_PLACEMENT_3D('',#11762,#9284,#9285);
#8190=AXIS2_PLACEMENT_3D('',#11765,#9287,#9288);
#8191=AXIS2_PLACEMENT_3D('',#11766,#9289,#9290);
#8192=AXIS2_PLACEMENT_3D('',#11768,#9291,#9292);
#8193=AXIS2_PLACEMENT_3D('',#11771,#9294,#9295);
#8194=AXIS2_PLACEMENT_3D('',#11772,#9296,#9297);
#8195=AXIS2_PLACEMENT_3D('',#11774,#9298,#9299);
#8196=AXIS2_PLACEMENT_3D('',#11777,#9301,#9302);
#8197=AXIS2_PLACEMENT_3D('',#11778,#9303,#9304);
#8198=AXIS2_PLACEMENT_3D('',#11780,#9305,#9306);
#8199=AXIS2_PLACEMENT_3D('',#11783,#9308,#9309);
#8200=AXIS2_PLACEMENT_3D('',#11784,#9310,#9311);
#8201=AXIS2_PLACEMENT_3D('',#11788,#9313,#9314);
#8202=AXIS2_PLACEMENT_3D('',#11789,#9315,#9316);
#8203=AXIS2_PLACEMENT_3D('',#11791,#9317,#9318);
#8204=AXIS2_PLACEMENT_3D('',#11794,#9320,#9321);
#8205=AXIS2_PLACEMENT_3D('',#11795,#9322,#9323);
#8206=AXIS2_PLACEMENT_3D('',#11796,#9324,#9325);
#8207=AXIS2_PLACEMENT_3D('',#11798,#9326,#9327);
#8208=AXIS2_PLACEMENT_3D('',#11799,#9328,#9329);
#8209=AXIS2_PLACEMENT_3D('',#11804,#9331,#9332);
#8210=AXIS2_PLACEMENT_3D('',#11805,#9333,#9334);
#8211=AXIS2_PLACEMENT_3D('',#11806,#9335,#9336);
#8212=AXIS2_PLACEMENT_3D('',#11808,#9337,#9338);
#8213=AXIS2_PLACEMENT_3D('',#11810,#9340,#9341);
#8214=AXIS2_PLACEMENT_3D('',#11811,#9342,#9343);
#8215=AXIS2_PLACEMENT_3D('',#11813,#9344,#9345);
#8216=AXIS2_PLACEMENT_3D('',#11814,#9346,#9347);
#8217=AXIS2_PLACEMENT_3D('',#11816,#9348,#9349);
#8218=AXIS2_PLACEMENT_3D('',#11818,#9351,#9352);
#8219=AXIS2_PLACEMENT_3D('',#11820,#9353,#9354);
#8220=AXIS2_PLACEMENT_3D('',#11822,#9356,#9357);
#8221=AXIS2_PLACEMENT_3D('',#11831,#9362,#9363);
#8222=AXIS2_PLACEMENT_3D('',#11840,#9368,#9369);
#8223=AXIS2_PLACEMENT_3D('',#11846,#9373,#9374);
#8224=AXIS2_PLACEMENT_3D('',#11852,#9378,#9379);
#8225=AXIS2_PLACEMENT_3D('',#11855,#9382,#9383);
#8226=AXIS2_PLACEMENT_3D('',#11856,#9384,#9385);
#8227=AXIS2_PLACEMENT_3D('',#11858,#9386,#9387);
#8228=AXIS2_PLACEMENT_3D('',#11859,#9388,#9389);
#8229=AXIS2_PLACEMENT_3D('',#11862,#9391,#9392);
#8230=AXIS2_PLACEMENT_3D('',#11863,#9393,#9394);
#8231=AXIS2_PLACEMENT_3D('',#11864,#9395,#9396);
#8232=AXIS2_PLACEMENT_3D('',#11865,#9397,#9398);
#8233=AXIS2_PLACEMENT_3D('',#11866,#9399,#9400);
#8234=AXIS2_PLACEMENT_3D('',#11867,#9401,#9402);
#8235=AXIS2_PLACEMENT_3D('',#11869,#9403,#9404);
#8236=AXIS2_PLACEMENT_3D('',#11872,#9406,#9407);
#8237=AXIS2_PLACEMENT_3D('',#11873,#9408,#9409);
#8238=AXIS2_PLACEMENT_3D('',#11875,#9410,#9411);
#8239=AXIS2_PLACEMENT_3D('',#11878,#9413,#9414);
#8240=AXIS2_PLACEMENT_3D('',#11879,#9415,#9416);
#8241=AXIS2_PLACEMENT_3D('',#11881,#9417,#9418);
#8242=AXIS2_PLACEMENT_3D('',#11884,#9420,#9421);
#8243=AXIS2_PLACEMENT_3D('',#11885,#9422,#9423);
#8244=AXIS2_PLACEMENT_3D('',#11887,#9424,#9425);
#8245=AXIS2_PLACEMENT_3D('',#11890,#9427,#9428);
#8246=AXIS2_PLACEMENT_3D('',#11891,#9429,#9430);
#8247=AXIS2_PLACEMENT_3D('',#11893,#9431,#9432);
#8248=AXIS2_PLACEMENT_3D('',#11896,#9434,#9435);
#8249=AXIS2_PLACEMENT_3D('',#11897,#9436,#9437);
#8250=AXIS2_PLACEMENT_3D('',#11899,#9438,#9439);
#8251=AXIS2_PLACEMENT_3D('',#11900,#9440,#9441);
#8252=AXIS2_PLACEMENT_3D('',#11903,#9443,#9444);
#8253=AXIS2_PLACEMENT_3D('',#11904,#9445,#9446);
#8254=AXIS2_PLACEMENT_3D('',#11906,#9447,#9448);
#8255=AXIS2_PLACEMENT_3D('',#11909,#9450,#9451);
#8256=AXIS2_PLACEMENT_3D('',#11910,#9452,#9453);
#8257=AXIS2_PLACEMENT_3D('',#11911,#9454,#9455);
#8258=AXIS2_PLACEMENT_3D('',#11912,#9456,#9457);
#8259=AXIS2_PLACEMENT_3D('',#11913,#9458,#9459);
#8260=AXIS2_PLACEMENT_3D('',#11915,#9460,#9461);
#8261=AXIS2_PLACEMENT_3D('',#11918,#9463,#9464);
#8262=AXIS2_PLACEMENT_3D('',#11919,#9465,#9466);
#8263=AXIS2_PLACEMENT_3D('',#11921,#9467,#9468);
#8264=AXIS2_PLACEMENT_3D('',#11924,#9470,#9471);
#8265=AXIS2_PLACEMENT_3D('',#11925,#9472,#9473);
#8266=AXIS2_PLACEMENT_3D('',#11927,#9474,#9475);
#8267=AXIS2_PLACEMENT_3D('',#11930,#9477,#9478);
#8268=AXIS2_PLACEMENT_3D('',#11931,#9479,#9480);
#8269=AXIS2_PLACEMENT_3D('',#11933,#9481,#9482);
#8270=AXIS2_PLACEMENT_3D('',#11936,#9484,#9485);
#8271=AXIS2_PLACEMENT_3D('',#11937,#9486,#9487);
#8272=AXIS2_PLACEMENT_3D('',#11939,#9488,#9489);
#8273=AXIS2_PLACEMENT_3D('',#11942,#9491,#9492);
#8274=AXIS2_PLACEMENT_3D('',#11943,#9493,#9494);
#8275=AXIS2_PLACEMENT_3D('',#11945,#9495,#9496);
#8276=AXIS2_PLACEMENT_3D('',#11946,#9497,#9498);
#8277=AXIS2_PLACEMENT_3D('',#11948,#9499,#9500);
#8278=AXIS2_PLACEMENT_3D('',#11950,#9502,#9503);
#8279=AXIS2_PLACEMENT_3D('',#11952,#9504,#9505);
#8280=AXIS2_PLACEMENT_3D('',#11955,#9507,#9508);
#8281=AXIS2_PLACEMENT_3D('',#11956,#9509,#9510);
#8282=AXIS2_PLACEMENT_3D('',#11957,#9511,#9512);
#8283=AXIS2_PLACEMENT_3D('',#11958,#9513,#9514);
#8284=AXIS2_PLACEMENT_3D('',#11959,#9515,#9516);
#8285=AXIS2_PLACEMENT_3D('',#11961,#9517,#9518);
#8286=AXIS2_PLACEMENT_3D('',#11964,#9520,#9521);
#8287=AXIS2_PLACEMENT_3D('',#11965,#9522,#9523);
#8288=AXIS2_PLACEMENT_3D('',#11967,#9524,#9525);
#8289=AXIS2_PLACEMENT_3D('',#11970,#9527,#9528);
#8290=AXIS2_PLACEMENT_3D('',#11971,#9529,#9530);
#8291=AXIS2_PLACEMENT_3D('',#11973,#9531,#9532);
#8292=AXIS2_PLACEMENT_3D('',#11976,#9534,#9535);
#8293=AXIS2_PLACEMENT_3D('',#11977,#9536,#9537);
#8294=AXIS2_PLACEMENT_3D('',#11979,#9538,#9539);
#8295=AXIS2_PLACEMENT_3D('',#11982,#9541,#9542);
#8296=AXIS2_PLACEMENT_3D('',#11983,#9543,#9544);
#8297=AXIS2_PLACEMENT_3D('',#11987,#9546,#9547);
#8298=AXIS2_PLACEMENT_3D('',#11988,#9548,#9549);
#8299=AXIS2_PLACEMENT_3D('',#11990,#9550,#9551);
#8300=AXIS2_PLACEMENT_3D('',#11993,#9553,#9554);
#8301=AXIS2_PLACEMENT_3D('',#11994,#9555,#9556);
#8302=AXIS2_PLACEMENT_3D('',#11995,#9557,#9558);
#8303=AXIS2_PLACEMENT_3D('',#11997,#9559,#9560);
#8304=AXIS2_PLACEMENT_3D('',#11998,#9561,#9562);
#8305=AXIS2_PLACEMENT_3D('',#12003,#9564,#9565);
#8306=AXIS2_PLACEMENT_3D('',#12004,#9566,#9567);
#8307=AXIS2_PLACEMENT_3D('',#12005,#9568,#9569);
#8308=AXIS2_PLACEMENT_3D('',#12007,#9570,#9571);
#8309=AXIS2_PLACEMENT_3D('',#12009,#9573,#9574);
#8310=AXIS2_PLACEMENT_3D('',#12010,#9575,#9576);
#8311=AXIS2_PLACEMENT_3D('',#12012,#9577,#9578);
#8312=AXIS2_PLACEMENT_3D('',#12013,#9579,#9580);
#8313=AXIS2_PLACEMENT_3D('',#12015,#9581,#9582);
#8314=AXIS2_PLACEMENT_3D('',#12017,#9584,#9585);
#8315=AXIS2_PLACEMENT_3D('',#12019,#9586,#9587);
#8316=AXIS2_PLACEMENT_3D('',#12021,#9589,#9590);
#8317=AXIS2_PLACEMENT_3D('',#12030,#9595,#9596);
#8318=AXIS2_PLACEMENT_3D('',#12039,#9601,#9602);
#8319=AXIS2_PLACEMENT_3D('',#12045,#9606,#9607);
#8320=AXIS2_PLACEMENT_3D('',#12051,#9611,#9612);
#8321=AXIS2_PLACEMENT_3D('',#12054,#9615,#9616);
#8322=AXIS2_PLACEMENT_3D('',#12055,#9617,#9618);
#8323=AXIS2_PLACEMENT_3D('',#12057,#9619,#9620);
#8324=AXIS2_PLACEMENT_3D('',#12058,#9621,#9622);
#8325=AXIS2_PLACEMENT_3D('',#12061,#9624,#9625);
#8326=AXIS2_PLACEMENT_3D('',#12062,#9626,#9627);
#8327=AXIS2_PLACEMENT_3D('',#12063,#9628,#9629);
#8328=AXIS2_PLACEMENT_3D('',#12064,#9630,#9631);
#8329=AXIS2_PLACEMENT_3D('',#12065,#9632,#9633);
#8330=AXIS2_PLACEMENT_3D('',#12066,#9634,#9635);
#8331=AXIS2_PLACEMENT_3D('',#12068,#9636,#9637);
#8332=AXIS2_PLACEMENT_3D('',#12071,#9639,#9640);
#8333=AXIS2_PLACEMENT_3D('',#12072,#9641,#9642);
#8334=AXIS2_PLACEMENT_3D('',#12074,#9643,#9644);
#8335=AXIS2_PLACEMENT_3D('',#12077,#9646,#9647);
#8336=AXIS2_PLACEMENT_3D('',#12078,#9648,#9649);
#8337=AXIS2_PLACEMENT_3D('',#12080,#9650,#9651);
#8338=AXIS2_PLACEMENT_3D('',#12083,#9653,#9654);
#8339=AXIS2_PLACEMENT_3D('',#12084,#9655,#9656);
#8340=AXIS2_PLACEMENT_3D('',#12086,#9657,#9658);
#8341=AXIS2_PLACEMENT_3D('',#12089,#9660,#9661);
#8342=AXIS2_PLACEMENT_3D('',#12090,#9662,#9663);
#8343=AXIS2_PLACEMENT_3D('',#12092,#9664,#9665);
#8344=AXIS2_PLACEMENT_3D('',#12095,#9667,#9668);
#8345=AXIS2_PLACEMENT_3D('',#12096,#9669,#9670);
#8346=AXIS2_PLACEMENT_3D('',#12098,#9671,#9672);
#8347=AXIS2_PLACEMENT_3D('',#12099,#9673,#9674);
#8348=AXIS2_PLACEMENT_3D('',#12102,#9676,#9677);
#8349=AXIS2_PLACEMENT_3D('',#12103,#9678,#9679);
#8350=AXIS2_PLACEMENT_3D('',#12105,#9680,#9681);
#8351=AXIS2_PLACEMENT_3D('',#12108,#9683,#9684);
#8352=AXIS2_PLACEMENT_3D('',#12109,#9685,#9686);
#8353=AXIS2_PLACEMENT_3D('',#12110,#9687,#9688);
#8354=AXIS2_PLACEMENT_3D('',#12111,#9689,#9690);
#8355=AXIS2_PLACEMENT_3D('',#12112,#9691,#9692);
#8356=AXIS2_PLACEMENT_3D('',#12114,#9693,#9694);
#8357=AXIS2_PLACEMENT_3D('',#12117,#9696,#9697);
#8358=AXIS2_PLACEMENT_3D('',#12118,#9698,#9699);
#8359=AXIS2_PLACEMENT_3D('',#12120,#9700,#9701);
#8360=AXIS2_PLACEMENT_3D('',#12123,#9703,#9704);
#8361=AXIS2_PLACEMENT_3D('',#12124,#9705,#9706);
#8362=AXIS2_PLACEMENT_3D('',#12126,#9707,#9708);
#8363=AXIS2_PLACEMENT_3D('',#12129,#9710,#9711);
#8364=AXIS2_PLACEMENT_3D('',#12130,#9712,#9713);
#8365=AXIS2_PLACEMENT_3D('',#12132,#9714,#9715);
#8366=AXIS2_PLACEMENT_3D('',#12135,#9717,#9718);
#8367=AXIS2_PLACEMENT_3D('',#12136,#9719,#9720);
#8368=AXIS2_PLACEMENT_3D('',#12138,#9721,#9722);
#8369=AXIS2_PLACEMENT_3D('',#12141,#9724,#9725);
#8370=AXIS2_PLACEMENT_3D('',#12142,#9726,#9727);
#8371=AXIS2_PLACEMENT_3D('',#12144,#9728,#9729);
#8372=AXIS2_PLACEMENT_3D('',#12145,#9730,#9731);
#8373=AXIS2_PLACEMENT_3D('',#12147,#9732,#9733);
#8374=AXIS2_PLACEMENT_3D('',#12149,#9735,#9736);
#8375=AXIS2_PLACEMENT_3D('',#12151,#9737,#9738);
#8376=AXIS2_PLACEMENT_3D('',#12154,#9740,#9741);
#8377=AXIS2_PLACEMENT_3D('',#12155,#9742,#9743);
#8378=AXIS2_PLACEMENT_3D('',#12156,#9744,#9745);
#8379=AXIS2_PLACEMENT_3D('',#12157,#9746,#9747);
#8380=AXIS2_PLACEMENT_3D('',#12158,#9748,#9749);
#8381=AXIS2_PLACEMENT_3D('',#12160,#9750,#9751);
#8382=AXIS2_PLACEMENT_3D('',#12163,#9753,#9754);
#8383=AXIS2_PLACEMENT_3D('',#12164,#9755,#9756);
#8384=AXIS2_PLACEMENT_3D('',#12166,#9757,#9758);
#8385=AXIS2_PLACEMENT_3D('',#12169,#9760,#9761);
#8386=AXIS2_PLACEMENT_3D('',#12170,#9762,#9763);
#8387=AXIS2_PLACEMENT_3D('',#12172,#9764,#9765);
#8388=AXIS2_PLACEMENT_3D('',#12175,#9767,#9768);
#8389=AXIS2_PLACEMENT_3D('',#12176,#9769,#9770);
#8390=AXIS2_PLACEMENT_3D('',#12178,#9771,#9772);
#8391=AXIS2_PLACEMENT_3D('',#12181,#9774,#9775);
#8392=AXIS2_PLACEMENT_3D('',#12182,#9776,#9777);
#8393=AXIS2_PLACEMENT_3D('',#12191,#9782,#9783);
#8394=AXIS2_PLACEMENT_3D('',#12193,#9784,#9785);
#8395=AXIS2_PLACEMENT_3D('',#12197,#9788,#9789);
#8396=AXIS2_PLACEMENT_3D('',#12199,#9790,#9791);
#8397=AXIS2_PLACEMENT_3D('',#12203,#9794,#9795);
#8398=AXIS2_PLACEMENT_3D('',#12206,#9798,#9799);
#8399=AXIS2_PLACEMENT_3D('',#12207,#9800,#9801);
#8400=AXIS2_PLACEMENT_3D('',#12209,#9802,#9803);
#8401=AXIS2_PLACEMENT_3D('',#12212,#9805,#9806);
#8402=AXIS2_PLACEMENT_3D('',#12213,#9807,#9808);
#8403=AXIS2_PLACEMENT_3D('',#12215,#9809,#9810);
#8404=AXIS2_PLACEMENT_3D('',#12218,#9812,#9813);
#8405=AXIS2_PLACEMENT_3D('',#12219,#9814,#9815);
#8406=AXIS2_PLACEMENT_3D('',#12220,#9816,#9817);
#8407=AXIS2_PLACEMENT_3D('',#12221,#9818,#9819);
#8408=AXIS2_PLACEMENT_3D('',#12222,#9820,#9821);
#8409=AXIS2_PLACEMENT_3D('',#12224,#9822,#9823);
#8410=AXIS2_PLACEMENT_3D('',#12227,#9825,#9826);
#8411=AXIS2_PLACEMENT_3D('',#12228,#9827,#9828);
#8412=AXIS2_PLACEMENT_3D('',#12230,#9829,#9830);
#8413=AXIS2_PLACEMENT_3D('',#12233,#9832,#9833);
#8414=AXIS2_PLACEMENT_3D('',#12234,#9834,#9835);
#8415=AXIS2_PLACEMENT_3D('',#12236,#9836,#9837);
#8416=AXIS2_PLACEMENT_3D('',#12239,#9839,#9840);
#8417=AXIS2_PLACEMENT_3D('',#12240,#9841,#9842);
#8418=AXIS2_PLACEMENT_3D('',#12242,#9843,#9844);
#8419=AXIS2_PLACEMENT_3D('',#12245,#9846,#9847);
#8420=AXIS2_PLACEMENT_3D('',#12246,#9848,#9849);
#8421=AXIS2_PLACEMENT_3D('',#12248,#9850,#9851);
#8422=AXIS2_PLACEMENT_3D('',#12251,#9853,#9854);
#8423=AXIS2_PLACEMENT_3D('',#12252,#9855,#9856);
#8424=AXIS2_PLACEMENT_3D('',#12254,#9857,#9858);
#8425=AXIS2_PLACEMENT_3D('',#12255,#9859,#9860);
#8426=AXIS2_PLACEMENT_3D('',#12258,#9862,#9863);
#8427=AXIS2_PLACEMENT_3D('',#12259,#9864,#9865);
#8428=AXIS2_PLACEMENT_3D('',#12261,#9866,#9867);
#8429=AXIS2_PLACEMENT_3D('',#12264,#9869,#9870);
#8430=AXIS2_PLACEMENT_3D('',#12265,#9871,#9872);
#8431=AXIS2_PLACEMENT_3D('',#12266,#9873,#9874);
#8432=AXIS2_PLACEMENT_3D('',#12267,#9875,#9876);
#8433=AXIS2_PLACEMENT_3D('',#12268,#9877,#9878);
#8434=AXIS2_PLACEMENT_3D('',#12270,#9879,#9880);
#8435=AXIS2_PLACEMENT_3D('',#12273,#9882,#9883);
#8436=AXIS2_PLACEMENT_3D('',#12274,#9884,#9885);
#8437=AXIS2_PLACEMENT_3D('',#12276,#9886,#9887);
#8438=AXIS2_PLACEMENT_3D('',#12279,#9889,#9890);
#8439=AXIS2_PLACEMENT_3D('',#12280,#9891,#9892);
#8440=AXIS2_PLACEMENT_3D('',#12282,#9893,#9894);
#8441=AXIS2_PLACEMENT_3D('',#12285,#9896,#9897);
#8442=AXIS2_PLACEMENT_3D('',#12286,#9898,#9899);
#8443=AXIS2_PLACEMENT_3D('',#12288,#9900,#9901);
#8444=AXIS2_PLACEMENT_3D('',#12291,#9903,#9904);
#8445=AXIS2_PLACEMENT_3D('',#12292,#9905,#9906);
#8446=AXIS2_PLACEMENT_3D('',#12294,#9907,#9908);
#8447=AXIS2_PLACEMENT_3D('',#12297,#9910,#9911);
#8448=AXIS2_PLACEMENT_3D('',#12298,#9912,#9913);
#8449=AXIS2_PLACEMENT_3D('',#12300,#9914,#9915);
#8450=AXIS2_PLACEMENT_3D('',#12301,#9916,#9917);
#8451=AXIS2_PLACEMENT_3D('',#12303,#9918,#9919);
#8452=AXIS2_PLACEMENT_3D('',#12305,#9921,#9922);
#8453=AXIS2_PLACEMENT_3D('',#12307,#9923,#9924);
#8454=AXIS2_PLACEMENT_3D('',#12310,#9926,#9927);
#8455=AXIS2_PLACEMENT_3D('',#12311,#9928,#9929);
#8456=AXIS2_PLACEMENT_3D('',#12312,#9930,#9931);
#8457=AXIS2_PLACEMENT_3D('',#12313,#9932,#9933);
#8458=AXIS2_PLACEMENT_3D('',#12314,#9934,#9935);
#8459=AXIS2_PLACEMENT_3D('',#12316,#9936,#9937);
#8460=AXIS2_PLACEMENT_3D('',#12319,#9939,#9940);
#8461=AXIS2_PLACEMENT_3D('',#12320,#9941,#9942);
#8462=AXIS2_PLACEMENT_3D('',#12321,#9943,#9944);
#8463=AXIS2_PLACEMENT_3D('',#12323,#9945,#9946);
#8464=AXIS2_PLACEMENT_3D('',#12326,#9948,#9949);
#8465=AXIS2_PLACEMENT_3D('',#12327,#9950,#9951);
#8466=AXIS2_PLACEMENT_3D('',#12328,#9952,#9953);
#8467=AXIS2_PLACEMENT_3D('',#12330,#9954,#9955);
#8468=AXIS2_PLACEMENT_3D('',#12333,#9957,#9958);
#8469=AXIS2_PLACEMENT_3D('',#12334,#9959,#9960);
#8470=AXIS2_PLACEMENT_3D('',#12336,#9961,#9962);
#8471=AXIS2_PLACEMENT_3D('',#12337,#9963,#9964);
#8472=AXIS2_PLACEMENT_3D('',#12339,#9965,#9966);
#8473=AXIS2_PLACEMENT_3D('',#12342,#9968,#9969);
#8474=AXIS2_PLACEMENT_3D('',#12343,#9970,#9971);
#8475=AXIS2_PLACEMENT_3D('',#12345,#9972,#9973);
#8476=AXIS2_PLACEMENT_3D('',#12346,#9974,#9975);
#8477=AXIS2_PLACEMENT_3D('',#12348,#9976,#9977);
#8478=AXIS2_PLACEMENT_3D('',#12351,#9979,#9980);
#8479=AXIS2_PLACEMENT_3D('',#12352,#9981,#9982);
#8480=AXIS2_PLACEMENT_3D('',#12354,#9983,#9984);
#8481=AXIS2_PLACEMENT_3D('',#12355,#9985,#9986);
#8482=AXIS2_PLACEMENT_3D('',#12357,#9987,#9988);
#8483=AXIS2_PLACEMENT_3D('',#12360,#9990,#9991);
#8484=AXIS2_PLACEMENT_3D('',#12361,#9992,#9993);
#8485=AXIS2_PLACEMENT_3D('',#12363,#9994,#9995);
#8486=AXIS2_PLACEMENT_3D('',#12364,#9996,#9997);
#8487=AXIS2_PLACEMENT_3D('',#12366,#9998,#9999);
#8488=AXIS2_PLACEMENT_3D('',#12368,#10001,#10002);
#8489=AXIS2_PLACEMENT_3D('',#12370,#10003,#10004);
#8490=AXIS2_PLACEMENT_3D('',#12372,#10006,#10007);
#8491=AXIS2_PLACEMENT_3D('',#12374,#10008,#10009);
#8492=AXIS2_PLACEMENT_3D('',#12376,#10011,#10012);
#8493=AXIS2_PLACEMENT_3D('',#12378,#10013,#10014);
#8494=AXIS2_PLACEMENT_3D('',#12380,#10016,#10017);
#8495=AXIS2_PLACEMENT_3D('',#12389,#10022,#10023);
#8496=AXIS2_PLACEMENT_3D('',#12395,#10027,#10028);
#8497=AXIS2_PLACEMENT_3D('',#12401,#10032,#10033);
#8498=AXIS2_PLACEMENT_3D('',#12404,#10036,#10037);
#8499=AXIS2_PLACEMENT_3D('',#12405,#10038,#10039);
#8500=AXIS2_PLACEMENT_3D('',#12406,#10040,#10041);
#8501=AXIS2_PLACEMENT_3D('',#12407,#10042,#10043);
#8502=AXIS2_PLACEMENT_3D('',#12409,#10044,#10045);
#8503=AXIS2_PLACEMENT_3D('',#12412,#10047,#10048);
#8504=AXIS2_PLACEMENT_3D('',#12413,#10049,#10050);
#8505=AXIS2_PLACEMENT_3D('',#12415,#10051,#10052);
#8506=AXIS2_PLACEMENT_3D('',#12418,#10054,#10055);
#8507=AXIS2_PLACEMENT_3D('',#12419,#10056,#10057);
#8508=AXIS2_PLACEMENT_3D('',#12428,#10062,#10063);
#8509=AXIS2_PLACEMENT_3D('',#12434,#10067,#10068);
#8510=AXIS2_PLACEMENT_3D('',#12440,#10072,#10073);
#8511=AXIS2_PLACEMENT_3D('',#12449,#10078,#10079);
#8512=AXIS2_PLACEMENT_3D('',#12455,#10083,#10084);
#8513=AXIS2_PLACEMENT_3D('',#12460,#10088,#10089);
#8514=AXIS2_PLACEMENT_3D('',#12464,#10092,#10093);
#8515=AXIS2_PLACEMENT_3D('',#12467,#10096,#10097);
#8516=AXIS2_PLACEMENT_3D('',#12468,#10098,#10099);
#8517=AXIS2_PLACEMENT_3D('',#12469,#10100,#10101);
#8518=AXIS2_PLACEMENT_3D('',#12470,#10102,#10103);
#8519=AXIS2_PLACEMENT_3D('',#12472,#10104,#10105);
#8520=AXIS2_PLACEMENT_3D('',#12475,#10107,#10108);
#8521=AXIS2_PLACEMENT_3D('',#12476,#10109,#10110);
#8522=AXIS2_PLACEMENT_3D('',#12478,#10111,#10112);
#8523=AXIS2_PLACEMENT_3D('',#12479,#10113,#10114);
#8524=AXIS2_PLACEMENT_3D('',#12481,#10115,#10116);
#8525=AXIS2_PLACEMENT_3D('',#12483,#10118,#10119);
#8526=AXIS2_PLACEMENT_3D('',#12485,#10120,#10121);
#8527=AXIS2_PLACEMENT_3D('',#12494,#10126,#10127);
#8528=AXIS2_PLACEMENT_3D('',#12497,#10129,#10130);
#8529=AXIS2_PLACEMENT_3D('',#12498,#10131,#10132);
#8530=AXIS2_PLACEMENT_3D('',#12512,#10140,#10141);
#8531=AXIS2_PLACEMENT_3D('',#12524,#10148,#10149);
#8532=AXIS2_PLACEMENT_3D('',#12526,#10150,#10151);
#8533=AXIS2_PLACEMENT_3D('',#12529,#10153,#10154);
#8534=AXIS2_PLACEMENT_3D('',#12530,#10155,#10156);
#8535=AXIS2_PLACEMENT_3D('',#12532,#10157,#10158);
#8536=AXIS2_PLACEMENT_3D('',#12533,#10159,#10160);
#8537=AXIS2_PLACEMENT_3D('',#12535,#10161,#10162);
#8538=AXIS2_PLACEMENT_3D('',#12537,#10164,#10165);
#8539=AXIS2_PLACEMENT_3D('',#12539,#10166,#10167);
#8540=AXIS2_PLACEMENT_3D('',#12545,#10171,#10172);
#8541=AXIS2_PLACEMENT_3D('',#12548,#10174,#10175);
#8542=AXIS2_PLACEMENT_3D('',#12549,#10176,#10177);
#8543=AXIS2_PLACEMENT_3D('',#12553,#10180,#10181);
#8544=AXIS2_PLACEMENT_3D('',#12557,#10184,#10185);
#8545=AXIS2_PLACEMENT_3D('',#12559,#10186,#10187);
#8546=AXIS2_PLACEMENT_3D('',#12562,#10189,#10190);
#8547=AXIS2_PLACEMENT_3D('',#12563,#10191,#10192);
#8548=AXIS2_PLACEMENT_3D('',#12565,#10193,#10194);
#8549=AXIS2_PLACEMENT_3D('',#12566,#10195,#10196);
#8550=AXIS2_PLACEMENT_3D('',#12568,#10197,#10198);
#8551=AXIS2_PLACEMENT_3D('',#12570,#10200,#10201);
#8552=AXIS2_PLACEMENT_3D('',#12572,#10202,#10203);
#8553=AXIS2_PLACEMENT_3D('',#12578,#10207,#10208);
#8554=AXIS2_PLACEMENT_3D('',#12581,#10210,#10211);
#8555=AXIS2_PLACEMENT_3D('',#12582,#10212,#10213);
#8556=AXIS2_PLACEMENT_3D('',#12588,#10217,#10218);
#8557=AXIS2_PLACEMENT_3D('',#12590,#10220,#10221);
#8558=AXIS2_PLACEMENT_3D('',#12592,#10222,#10223);
#8559=AXIS2_PLACEMENT_3D('',#12595,#10225,#10226);
#8560=AXIS2_PLACEMENT_3D('',#12596,#10227,#10228);
#8561=AXIS2_PLACEMENT_3D('',#12598,#10229,#10230);
#8562=AXIS2_PLACEMENT_3D('',#12599,#10231,#10232);
#8563=AXIS2_PLACEMENT_3D('',#12601,#10233,#10234);
#8564=AXIS2_PLACEMENT_3D('',#12603,#10236,#10237);
#8565=AXIS2_PLACEMENT_3D('',#12605,#10238,#10239);
#8566=AXIS2_PLACEMENT_3D('',#12614,#10244,#10245);
#8567=AXIS2_PLACEMENT_3D('',#12617,#10247,#10248);
#8568=AXIS2_PLACEMENT_3D('',#12618,#10249,#10250);
#8569=AXIS2_PLACEMENT_3D('',#12625,#10255,#10256);
#8570=AXIS2_PLACEMENT_3D('',#12629,#10259,#10260);
#8571=AXIS2_PLACEMENT_3D('',#12638,#10265,#10266);
#8572=AXIS2_PLACEMENT_3D('',#12644,#10270,#10271);
#8573=AXIS2_PLACEMENT_3D('',#12650,#10275,#10276);
#8574=AXIS2_PLACEMENT_3D('',#12653,#10279,#10280);
#8575=AXIS2_PLACEMENT_3D('',#12657,#10283,#10284);
#8576=AXIS2_PLACEMENT_3D('',#12658,#10285,#10286);
#8577=AXIS2_PLACEMENT_3D('',#12660,#10288,#10289);
#8578=AXIS2_PLACEMENT_3D('',#12664,#10292,#10293);
#8579=AXIS2_PLACEMENT_3D('',#12665,#10294,#10295);
#8580=AXIS2_PLACEMENT_3D('',#12666,#10296,#10297);
#8581=AXIS2_PLACEMENT_3D('',#12668,#10299,#10300);
#8582=AXIS2_PLACEMENT_3D('',#12669,#10301,#10302);
#8583=AXIS2_PLACEMENT_3D('',#12671,#10304,#10305);
#8584=AXIS2_PLACEMENT_3D('',#12672,#10306,#10307);
#8585=AXIS2_PLACEMENT_3D('',#12673,#10308,#10309);
#8586=AXIS2_PLACEMENT_3D('',#12682,#10314,#10315);
#8587=AXIS2_PLACEMENT_3D('',#12688,#10319,#10320);
#8588=AXIS2_PLACEMENT_3D('',#12694,#10324,#10325);
#8589=AXIS2_PLACEMENT_3D('',#12697,#10328,#10329);
#8590=AXIS2_PLACEMENT_3D('',#12698,#10330,#10331);
#8591=AXIS2_PLACEMENT_3D('',#12699,#10332,#10333);
#8592=AXIS2_PLACEMENT_3D('',#12700,#10334,#10335);
#8593=AXIS2_PLACEMENT_3D('',#12709,#10340,#10341);
#8594=AXIS2_PLACEMENT_3D('',#12715,#10345,#10346);
#8595=AXIS2_PLACEMENT_3D('',#12721,#10350,#10351);
#8596=AXIS2_PLACEMENT_3D('',#12724,#10354,#10355);
#8597=AXIS2_PLACEMENT_3D('',#12725,#10356,#10357);
#8598=AXIS2_PLACEMENT_3D('',#12726,#10358,#10359);
#8599=AXIS2_PLACEMENT_3D('',#12727,#10360,#10361);
#8600=AXIS2_PLACEMENT_3D('',#12736,#10366,#10367);
#8601=AXIS2_PLACEMENT_3D('',#12742,#10371,#10372);
#8602=AXIS2_PLACEMENT_3D('',#12748,#10376,#10377);
#8603=AXIS2_PLACEMENT_3D('',#12754,#10381,#10382);
#8604=AXIS2_PLACEMENT_3D('',#12760,#10386,#10387);
#8605=AXIS2_PLACEMENT_3D('',#12763,#10390,#10391);
#8606=AXIS2_PLACEMENT_3D('',#12764,#10392,#10393);
#8607=AXIS2_PLACEMENT_3D('',#12765,#10394,#10395);
#8608=AXIS2_PLACEMENT_3D('',#12767,#10396,#10397);
#8609=AXIS2_PLACEMENT_3D('',#12768,#10398,#10399);
#8610=AXIS2_PLACEMENT_3D('',#12770,#10400,#10401);
#8611=AXIS2_PLACEMENT_3D('',#12771,#10402,#10403);
#8612=AXIS2_PLACEMENT_3D('',#12773,#10404,#10405);
#8613=AXIS2_PLACEMENT_3D('',#12775,#10407,#10408);
#8614=AXIS2_PLACEMENT_3D('',#12777,#10409,#10410);
#8615=AXIS2_PLACEMENT_3D('',#12779,#10412,#10413);
#8616=AXIS2_PLACEMENT_3D('',#12781,#10414,#10415);
#8617=AXIS2_PLACEMENT_3D('',#12783,#10417,#10418);
#8618=AXIS2_PLACEMENT_3D('',#12785,#10419,#10420);
#8619=AXIS2_PLACEMENT_3D('',#12786,#10421,#10422);
#8620=AXIS2_PLACEMENT_3D('',#12788,#10423,#10424);
#8621=AXIS2_PLACEMENT_3D('',#12790,#10426,#10427);
#8622=AXIS2_PLACEMENT_3D('',#12792,#10429,#10430);
#8623=AXIS2_PLACEMENT_3D('',#12793,#10431,#10432);
#8624=AXIS2_PLACEMENT_3D('',#12794,#10433,#10434);
#8625=AXIS2_PLACEMENT_3D('',#12797,#10435,#10436);
#8626=AXIS2_PLACEMENT_3D('',#12798,#10437,#10438);
#8627=AXIS2_PLACEMENT_3D('',#12800,#10439,#10440);
#8628=AXIS2_PLACEMENT_3D('',#12802,#10441,#10442);
#8629=AXIS2_PLACEMENT_3D('',#12803,#10443,#10444);
#8630=AXIS2_PLACEMENT_3D('',#12804,#10445,#10446);
#8631=AXIS2_PLACEMENT_3D('',#12807,#10448,#10449);
#8632=AXIS2_PLACEMENT_3D('',#12808,#10450,#10451);
#8633=AXIS2_PLACEMENT_3D('',#12810,#10452,#10453);
#8634=AXIS2_PLACEMENT_3D('',#12813,#10455,#10456);
#8635=AXIS2_PLACEMENT_3D('',#12814,#10457,#10458);
#8636=AXIS2_PLACEMENT_3D('',#12817,#10460,#10461);
#8637=AXIS2_PLACEMENT_3D('',#12818,#10462,#10463);
#8638=AXIS2_PLACEMENT_3D('',#12819,#10464,#10465);
#8639=AXIS2_PLACEMENT_3D('',#12821,#10466,#10467);
#8640=AXIS2_PLACEMENT_3D('',#12823,#10469,#10470);
#8641=AXIS2_PLACEMENT_3D('',#12825,#10471,#10472);
#8642=AXIS2_PLACEMENT_3D('',#12826,#10473,#10474);
#8643=AXIS2_PLACEMENT_3D('',#12828,#10476,#10477);
#8644=AXIS2_PLACEMENT_3D('',#12829,#10478,#10479);
#8645=AXIS2_PLACEMENT_3D('',#12832,#10480,#10481);
#8646=AXIS2_PLACEMENT_3D('',#12833,#10482,#10483);
#8647=AXIS2_PLACEMENT_3D('',#12835,#10484,#10485);
#8648=AXIS2_PLACEMENT_3D('',#12837,#10486,#10487);
#8649=AXIS2_PLACEMENT_3D('',#12838,#10488,#10489);
#8650=AXIS2_PLACEMENT_3D('',#12839,#10490,#10491);
#8651=AXIS2_PLACEMENT_3D('',#12841,#10492,#10493);
#8652=AXIS2_PLACEMENT_3D('',#12843,#10495,#10496);
#8653=AXIS2_PLACEMENT_3D('',#12845,#10497,#10498);
#8654=AXIS2_PLACEMENT_3D('',#12847,#10499,#10500);
#8655=AXIS2_PLACEMENT_3D('',#12848,#10501,#10502);
#8656=AXIS2_PLACEMENT_3D('',#12850,#10503,#10504);
#8657=AXIS2_PLACEMENT_3D('',#12852,#10506,#10507);
#8658=AXIS2_PLACEMENT_3D('',#12854,#10508,#10509);
#8659=AXIS2_PLACEMENT_3D('',#12856,#10511,#10512);
#8660=AXIS2_PLACEMENT_3D('',#12858,#10513,#10514);
#8661=AXIS2_PLACEMENT_3D('',#12860,#10516,#10517);
#8662=AXIS2_PLACEMENT_3D('',#12861,#10518,#10519);
#8663=AXIS2_PLACEMENT_3D('',#12863,#10521,#10522);
#8664=AXIS2_PLACEMENT_3D('',#12864,#10523,#10524);
#8665=AXIS2_PLACEMENT_3D('',#12867,#10525,#10526);
#8666=AXIS2_PLACEMENT_3D('',#12868,#10527,#10528);
#8667=AXIS2_PLACEMENT_3D('',#12871,#10529,#10530);
#8668=AXIS2_PLACEMENT_3D('',#12872,#10531,#10532);
#8669=AXIS2_PLACEMENT_3D('',#12875,#10533,#10534);
#8670=AXIS2_PLACEMENT_3D('',#12876,#10535,#10536);
#8671=AXIS2_PLACEMENT_3D('',#12879,#10537,#10538);
#8672=AXIS2_PLACEMENT_3D('',#12880,#10539,#10540);
#8673=AXIS2_PLACEMENT_3D('',#12883,#10541,#10542);
#8674=AXIS2_PLACEMENT_3D('',#12884,#10543,#10544);
#8675=AXIS2_PLACEMENT_3D('',#12887,#10545,#10546);
#8676=AXIS2_PLACEMENT_3D('',#12888,#10547,#10548);
#8677=AXIS2_PLACEMENT_3D('',#12891,#10549,#10550);
#8678=AXIS2_PLACEMENT_3D('',#12892,#10551,#10552);
#8679=AXIS2_PLACEMENT_3D('',#12893,#10553,#10554);
#8680=AXIS2_PLACEMENT_3D('',#12919,#10555,#10556);
#8681=AXIS2_PLACEMENT_3D('',#12943,#10557,#10558);
#8682=AXIS2_PLACEMENT_3D('',#12944,#10559,#10560);
#8683=AXIS2_PLACEMENT_3D('',#12946,#10561,#10562);
#8684=AXIS2_PLACEMENT_3D('',#12971,#10563,#10564);
#8685=AXIS2_PLACEMENT_3D('',#12996,#10565,#10566);
#8686=AXIS2_PLACEMENT_3D('',#12999,#10568,#10569);
#8687=AXIS2_PLACEMENT_3D('',#13001,#10570,#10571);
#8688=AXIS2_PLACEMENT_3D('',#13026,#10572,#10573);
#8689=AXIS2_PLACEMENT_3D('',#13051,#10574,#10575);
#8690=AXIS2_PLACEMENT_3D('',#13076,#10576,#10577);
#8691=AXIS2_PLACEMENT_3D('',#13100,#10578,#10579);
#8692=AXIS2_PLACEMENT_3D('',#13101,#10580,#10581);
#8693=AXIS2_PLACEMENT_3D('',#13103,#10582,#10583);
#8694=AXIS2_PLACEMENT_3D('',#13104,#10584,#10585);
#8695=AXIS2_PLACEMENT_3D('',#13105,#10586,#10587);
#8696=AXIS2_PLACEMENT_3D('',#13129,#10588,#10589);
#8697=AXIS2_PLACEMENT_3D('',#13130,#10590,#10591);
#8698=AXIS2_PLACEMENT_3D('',#13132,#10592,#10593);
#8699=AXIS2_PLACEMENT_3D('',#13133,#10594,#10595);
#8700=AXIS2_PLACEMENT_3D('',#13134,#10596,#10597);
#8701=AXIS2_PLACEMENT_3D('',#13158,#10598,#10599);
#8702=AXIS2_PLACEMENT_3D('',#13159,#10600,#10601);
#8703=AXIS2_PLACEMENT_3D('',#13161,#10602,#10603);
#8704=AXIS2_PLACEMENT_3D('',#13163,#10604,#10605);
#8705=AXIS2_PLACEMENT_3D('',#13164,#10606,#10607);
#8706=AXIS2_PLACEMENT_3D('',#13165,#10608,#10609);
#8707=AXIS2_PLACEMENT_3D('',#13189,#10610,#10611);
#8708=AXIS2_PLACEMENT_3D('',#13190,#10612,#10613);
#8709=AXIS2_PLACEMENT_3D('',#13192,#10614,#10615);
#8710=AXIS2_PLACEMENT_3D('',#13193,#10616,#10617);
#8711=AXIS2_PLACEMENT_3D('',#13194,#10618,#10619);
#8712=AXIS2_PLACEMENT_3D('',#13218,#10620,#10621);
#8713=AXIS2_PLACEMENT_3D('',#13219,#10622,#10623);
#8714=AXIS2_PLACEMENT_3D('',#13221,#10624,#10625);
#8715=AXIS2_PLACEMENT_3D('',#13222,#10626,#10627);
#8716=AXIS2_PLACEMENT_3D('',#13223,#10628,#10629);
#8717=AXIS2_PLACEMENT_3D('',#13247,#10630,#10631);
#8718=AXIS2_PLACEMENT_3D('',#13248,#10632,#10633);
#8719=AXIS2_PLACEMENT_3D('',#13250,#10634,#10635);
#8720=AXIS2_PLACEMENT_3D('',#13253,#10637,#10638);
#8721=AXIS2_PLACEMENT_3D('',#13277,#10639,#10640);
#8722=AXIS2_PLACEMENT_3D('',#13278,#10641,#10642);
#8723=AXIS2_PLACEMENT_3D('',#13279,#10643,#10644);
#8724=AXIS2_PLACEMENT_3D('',#13280,#10645,#10646);
#8725=AXIS2_PLACEMENT_3D('',#13281,#10647,#10648);
#8726=AXIS2_PLACEMENT_3D('',#13282,#10649,#10650);
#8727=AXIS2_PLACEMENT_3D('',#13283,#10651,#10652);
#8728=AXIS2_PLACEMENT_3D('',#13284,#10653,#10654);
#8729=AXIS2_PLACEMENT_3D('',#13285,#10655,#10656);
#8730=AXIS2_PLACEMENT_3D('',#13287,#10657,#10658);
#8731=AXIS2_PLACEMENT_3D('',#13289,#10659,#10660);
#8732=AXIS2_PLACEMENT_3D('',#13290,#10661,#10662);
#8733=AXIS2_PLACEMENT_3D('',#13292,#10663,#10664);
#8734=AXIS2_PLACEMENT_3D('',#13294,#10666,#10667);
#8735=AXIS2_PLACEMENT_3D('',#13296,#10668,#10669);
#8736=AXIS2_PLACEMENT_3D('',#13297,#10670,#10671);
#8737=AXIS2_PLACEMENT_3D('',#13299,#10673,#10674);
#8738=AXIS2_PLACEMENT_3D('',#13301,#10675,#10676);
#8739=AXIS2_PLACEMENT_3D('',#13303,#10677,#10678);
#8740=AXIS2_PLACEMENT_3D('',#13304,#10679,#10680);
#8741=AXIS2_PLACEMENT_3D('',#13306,#10681,#10682);
#8742=AXIS2_PLACEMENT_3D('',#13308,#10684,#10685);
#8743=AXIS2_PLACEMENT_3D('',#13310,#10686,#10687);
#8744=AXIS2_PLACEMENT_3D('',#13311,#10688,#10689);
#8745=AXIS2_PLACEMENT_3D('',#13313,#10691,#10692);
#8746=AXIS2_PLACEMENT_3D('',#13314,#10693,#10694);
#8747=AXIS2_PLACEMENT_3D('',#13315,#10695,#10696);
#8748=AXIS2_PLACEMENT_3D('',#13316,#10697,#10698);
#8749=AXIS2_PLACEMENT_3D('',#13317,#10699,#10700);
#8750=AXIS2_PLACEMENT_3D('',#13318,#10701,#10702);
#8751=AXIS2_PLACEMENT_3D('',#13319,#10703,#10704);
#8752=AXIS2_PLACEMENT_3D('',#13320,#10705,#10706);
#8753=AXIS2_PLACEMENT_3D('',#13323,#10707,#10708);
#8754=AXIS2_PLACEMENT_3D('',#13324,#10709,#10710);
#8755=AXIS2_PLACEMENT_3D('',#13326,#10711,#10712);
#8756=AXIS2_PLACEMENT_3D('',#13328,#10713,#10714);
#8757=AXIS2_PLACEMENT_3D('',#13329,#10715,#10716);
#8758=AXIS2_PLACEMENT_3D('',#13330,#10717,#10718);
#8759=AXIS2_PLACEMENT_3D('',#13333,#10720,#10721);
#8760=AXIS2_PLACEMENT_3D('',#13334,#10722,#10723);
#8761=AXIS2_PLACEMENT_3D('',#13336,#10724,#10725);
#8762=AXIS2_PLACEMENT_3D('',#13339,#10727,#10728);
#8763=AXIS2_PLACEMENT_3D('',#13340,#10729,#10730);
#8764=AXIS2_PLACEMENT_3D('',#13343,#10732,#10733);
#8765=AXIS2_PLACEMENT_3D('',#13344,#10734,#10735);
#8766=AXIS2_PLACEMENT_3D('',#13345,#10736,#10737);
#8767=AXIS2_PLACEMENT_3D('',#13347,#10738,#10739);
#8768=AXIS2_PLACEMENT_3D('',#13349,#10741,#10742);
#8769=AXIS2_PLACEMENT_3D('',#13351,#10743,#10744);
#8770=AXIS2_PLACEMENT_3D('',#13352,#10745,#10746);
#8771=AXIS2_PLACEMENT_3D('',#13354,#10748,#10749);
#8772=AXIS2_PLACEMENT_3D('',#13355,#10750,#10751);
#8773=AXIS2_PLACEMENT_3D('',#13358,#10752,#10753);
#8774=AXIS2_PLACEMENT_3D('',#13359,#10754,#10755);
#8775=AXIS2_PLACEMENT_3D('',#13361,#10756,#10757);
#8776=AXIS2_PLACEMENT_3D('',#13363,#10758,#10759);
#8777=AXIS2_PLACEMENT_3D('',#13364,#10760,#10761);
#8778=AXIS2_PLACEMENT_3D('',#13365,#10762,#10763);
#8779=AXIS2_PLACEMENT_3D('',#13367,#10764,#10765);
#8780=AXIS2_PLACEMENT_3D('',#13369,#10767,#10768);
#8781=AXIS2_PLACEMENT_3D('',#13371,#10769,#10770);
#8782=AXIS2_PLACEMENT_3D('',#13373,#10771,#10772);
#8783=AXIS2_PLACEMENT_3D('',#13374,#10773,#10774);
#8784=AXIS2_PLACEMENT_3D('',#13376,#10775,#10776);
#8785=AXIS2_PLACEMENT_3D('',#13378,#10778,#10779);
#8786=AXIS2_PLACEMENT_3D('',#13380,#10780,#10781);
#8787=AXIS2_PLACEMENT_3D('',#13382,#10783,#10784);
#8788=AXIS2_PLACEMENT_3D('',#13384,#10785,#10786);
#8789=AXIS2_PLACEMENT_3D('',#13386,#10788,#10789);
#8790=AXIS2_PLACEMENT_3D('',#13387,#10790,#10791);
#8791=AXIS2_PLACEMENT_3D('',#13389,#10793,#10794);
#8792=AXIS2_PLACEMENT_3D('',#13390,#10795,#10796);
#8793=AXIS2_PLACEMENT_3D('',#13393,#10797,#10798);
#8794=AXIS2_PLACEMENT_3D('',#13394,#10799,#10800);
#8795=AXIS2_PLACEMENT_3D('',#13397,#10801,#10802);
#8796=AXIS2_PLACEMENT_3D('',#13398,#10803,#10804);
#8797=AXIS2_PLACEMENT_3D('',#13401,#10805,#10806);
#8798=AXIS2_PLACEMENT_3D('',#13402,#10807,#10808);
#8799=AXIS2_PLACEMENT_3D('',#13405,#10809,#10810);
#8800=AXIS2_PLACEMENT_3D('',#13406,#10811,#10812);
#8801=AXIS2_PLACEMENT_3D('',#13409,#10813,#10814);
#8802=AXIS2_PLACEMENT_3D('',#13410,#10815,#10816);
#8803=AXIS2_PLACEMENT_3D('',#13413,#10817,#10818);
#8804=AXIS2_PLACEMENT_3D('',#13414,#10819,#10820);
#8805=AXIS2_PLACEMENT_3D('',#13417,#10821,#10822);
#8806=AXIS2_PLACEMENT_3D('',#13418,#10823,#10824);
#8807=AXIS2_PLACEMENT_3D('',#13421,#10825,#10826);
#8808=AXIS2_PLACEMENT_3D('',#13422,#10827,#10828);
#8809=AXIS2_PLACEMENT_3D('',#13423,#10829,#10830);
#8810=AXIS2_PLACEMENT_3D('',#13449,#10831,#10832);
#8811=AXIS2_PLACEMENT_3D('',#13473,#10833,#10834);
#8812=AXIS2_PLACEMENT_3D('',#13474,#10835,#10836);
#8813=AXIS2_PLACEMENT_3D('',#13476,#10837,#10838);
#8814=AXIS2_PLACEMENT_3D('',#13501,#10839,#10840);
#8815=AXIS2_PLACEMENT_3D('',#13526,#10841,#10842);
#8816=AXIS2_PLACEMENT_3D('',#13542,#10844,#10845);
#8817=AXIS2_PLACEMENT_3D('',#13557,#10846,#10847);
#8818=AXIS2_PLACEMENT_3D('',#13582,#10848,#10849);
#8819=AXIS2_PLACEMENT_3D('',#13607,#10850,#10851);
#8820=AXIS2_PLACEMENT_3D('',#13632,#10852,#10853);
#8821=AXIS2_PLACEMENT_3D('',#13656,#10854,#10855);
#8822=AXIS2_PLACEMENT_3D('',#13657,#10856,#10857);
#8823=AXIS2_PLACEMENT_3D('',#13659,#10858,#10859);
#8824=AXIS2_PLACEMENT_3D('',#13660,#10860,#10861);
#8825=AXIS2_PLACEMENT_3D('',#13661,#10862,#10863);
#8826=AXIS2_PLACEMENT_3D('',#13685,#10864,#10865);
#8827=AXIS2_PLACEMENT_3D('',#13686,#10866,#10867);
#8828=AXIS2_PLACEMENT_3D('',#13688,#10868,#10869);
#8829=AXIS2_PLACEMENT_3D('',#13689,#10870,#10871);
#8830=AXIS2_PLACEMENT_3D('',#13690,#10872,#10873);
#8831=AXIS2_PLACEMENT_3D('',#13714,#10874,#10875);
#8832=AXIS2_PLACEMENT_3D('',#13715,#10876,#10877);
#8833=AXIS2_PLACEMENT_3D('',#13717,#10878,#10879);
#8834=AXIS2_PLACEMENT_3D('',#13718,#10880,#10881);
#8835=AXIS2_PLACEMENT_3D('',#13719,#10882,#10883);
#8836=AXIS2_PLACEMENT_3D('',#13734,#10884,#10885);
#8837=AXIS2_PLACEMENT_3D('',#13747,#10886,#10887);
#8838=AXIS2_PLACEMENT_3D('',#13749,#10888,#10889);
#8839=AXIS2_PLACEMENT_3D('',#13750,#10890,#10891);
#8840=AXIS2_PLACEMENT_3D('',#13751,#10892,#10893);
#8841=AXIS2_PLACEMENT_3D('',#13775,#10894,#10895);
#8842=AXIS2_PLACEMENT_3D('',#13776,#10896,#10897);
#8843=AXIS2_PLACEMENT_3D('',#13778,#10898,#10899);
#8844=AXIS2_PLACEMENT_3D('',#13779,#10900,#10901);
#8845=AXIS2_PLACEMENT_3D('',#13780,#10902,#10903);
#8846=AXIS2_PLACEMENT_3D('',#13804,#10904,#10905);
#8847=AXIS2_PLACEMENT_3D('',#13805,#10906,#10907);
#8848=AXIS2_PLACEMENT_3D('',#13807,#10908,#10909);
#8849=AXIS2_PLACEMENT_3D('',#13808,#10910,#10911);
#8850=AXIS2_PLACEMENT_3D('',#13809,#10912,#10913);
#8851=AXIS2_PLACEMENT_3D('',#13833,#10914,#10915);
#8852=AXIS2_PLACEMENT_3D('',#13834,#10916,#10917);
#8853=AXIS2_PLACEMENT_3D('',#13836,#10918,#10919);
#8854=AXIS2_PLACEMENT_3D('',#13839,#10921,#10922);
#8855=AXIS2_PLACEMENT_3D('',#13863,#10923,#10924);
#8856=AXIS2_PLACEMENT_3D('',#13864,#10925,#10926);
#8857=AXIS2_PLACEMENT_3D('',#13865,#10927,#10928);
#8858=AXIS2_PLACEMENT_3D('',#13866,#10929,#10930);
#8859=AXIS2_PLACEMENT_3D('',#13867,#10931,#10932);
#8860=AXIS2_PLACEMENT_3D('',#13868,#10933,#10934);
#8861=AXIS2_PLACEMENT_3D('',#13869,#10935,#10936);
#8862=AXIS2_PLACEMENT_3D('',#13870,#10937,#10938);
#8863=AXIS2_PLACEMENT_3D('',#13871,#10939,#10940);
#8864=AXIS2_PLACEMENT_3D('',#13873,#10941,#10942);
#8865=AXIS2_PLACEMENT_3D('',#13875,#10943,#10944);
#8866=AXIS2_PLACEMENT_3D('',#13876,#10945,#10946);
#8867=AXIS2_PLACEMENT_3D('',#13878,#10947,#10948);
#8868=AXIS2_PLACEMENT_3D('',#13880,#10950,#10951);
#8869=AXIS2_PLACEMENT_3D('',#13882,#10952,#10953);
#8870=AXIS2_PLACEMENT_3D('',#13883,#10954,#10955);
#8871=AXIS2_PLACEMENT_3D('',#13885,#10957,#10958);
#8872=AXIS2_PLACEMENT_3D('',#13887,#10959,#10960);
#8873=AXIS2_PLACEMENT_3D('',#13889,#10961,#10962);
#8874=AXIS2_PLACEMENT_3D('',#13890,#10963,#10964);
#8875=AXIS2_PLACEMENT_3D('',#13892,#10965,#10966);
#8876=AXIS2_PLACEMENT_3D('',#13894,#10968,#10969);
#8877=AXIS2_PLACEMENT_3D('',#13896,#10970,#10971);
#8878=AXIS2_PLACEMENT_3D('',#13897,#10972,#10973);
#8879=AXIS2_PLACEMENT_3D('',#13899,#10975,#10976);
#8880=AXIS2_PLACEMENT_3D('',#13900,#10977,#10978);
#8881=AXIS2_PLACEMENT_3D('',#13901,#10979,#10980);
#8882=AXIS2_PLACEMENT_3D('',#13902,#10981,#10982);
#8883=AXIS2_PLACEMENT_3D('',#13903,#10983,#10984);
#8884=AXIS2_PLACEMENT_3D('',#13904,#10985,#10986);
#8885=AXIS2_PLACEMENT_3D('',#13905,#10987,#10988);
#8886=AXIS2_PLACEMENT_3D('',#13907,#10989,#10990);
#8887=AXIS2_PLACEMENT_3D('',#13908,#10991,#10992);
#8888=AXIS2_PLACEMENT_3D('',#13910,#10993,#10994);
#8889=AXIS2_PLACEMENT_3D('',#13912,#10996,#10997);
#8890=AXIS2_PLACEMENT_3D('',#13914,#10998,#10999);
#8891=AXIS2_PLACEMENT_3D('',#13916,#11001,#11002);
#8892=AXIS2_PLACEMENT_3D('',#13918,#11003,#11004);
#8893=AXIS2_PLACEMENT_3D('',#13920,#11006,#11007);
#8894=AXIS2_PLACEMENT_3D('',#13922,#11008,#11009);
#8895=AXIS2_PLACEMENT_3D('',#13923,#11010,#11011);
#8896=AXIS2_PLACEMENT_3D('',#13925,#11012,#11013);
#8897=AXIS2_PLACEMENT_3D('',#13927,#11015,#11016);
#8898=AXIS2_PLACEMENT_3D('',#13929,#11017,#11018);
#8899=AXIS2_PLACEMENT_3D('',#13931,#11020,#11021);
#8900=AXIS2_PLACEMENT_3D('',#13933,#11022,#11023);
#8901=AXIS2_PLACEMENT_3D('',#13935,#11025,#11026);
#8902=AXIS2_PLACEMENT_3D('',#13936,#11027,#11028);
#8903=AXIS2_PLACEMENT_3D('',#13945,#11033,#11034);
#8904=AXIS2_PLACEMENT_3D('',#13951,#11038,#11039);
#8905=AXIS2_PLACEMENT_3D('',#13957,#11043,#11044);
#8906=AXIS2_PLACEMENT_3D('',#13963,#11048,#11049);
#8907=AXIS2_PLACEMENT_3D('',#13969,#11053,#11054);
#8908=AXIS2_PLACEMENT_3D('',#13972,#11057,#11058);
#8909=AXIS2_PLACEMENT_3D('',#13973,#11059,#11060);
#8910=AXIS2_PLACEMENT_3D('',#13974,#11061,#11062);
#8911=AXIS2_PLACEMENT_3D('',#13975,#11063,#11064);
#8912=AXIS2_PLACEMENT_3D('',#13984,#11069,#11070);
#8913=AXIS2_PLACEMENT_3D('',#13990,#11074,#11075);
#8914=AXIS2_PLACEMENT_3D('',#13996,#11079,#11080);
#8915=AXIS2_PLACEMENT_3D('',#14002,#11084,#11085);
#8916=AXIS2_PLACEMENT_3D('',#14008,#11089,#11090);
#8917=AXIS2_PLACEMENT_3D('',#14011,#11093,#11094);
#8918=AXIS2_PLACEMENT_3D('',#14012,#11095,#11096);
#8919=AXIS2_PLACEMENT_3D('',#14013,#11097,#11098);
#8920=AXIS2_PLACEMENT_3D('',#14015,#11099,#11100);
#8921=AXIS2_PLACEMENT_3D('',#14016,#11101,#11102);
#8922=AXIS2_PLACEMENT_3D('',#14018,#11103,#11104);
#8923=AXIS2_PLACEMENT_3D('',#14019,#11105,#11106);
#8924=AXIS2_PLACEMENT_3D('',#14021,#11107,#11108);
#8925=AXIS2_PLACEMENT_3D('',#14023,#11110,#11111);
#8926=AXIS2_PLACEMENT_3D('',#14025,#11112,#11113);
#8927=AXIS2_PLACEMENT_3D('',#14027,#11115,#11116);
#8928=AXIS2_PLACEMENT_3D('',#14029,#11117,#11118);
#8929=AXIS2_PLACEMENT_3D('',#14031,#11120,#11121);
#8930=AXIS2_PLACEMENT_3D('',#14033,#11122,#11123);
#8931=AXIS2_PLACEMENT_3D('',#14034,#11124,#11125);
#8932=AXIS2_PLACEMENT_3D('',#14036,#11126,#11127);
#8933=AXIS2_PLACEMENT_3D('',#14038,#11129,#11130);
#8934=AXIS2_PLACEMENT_3D('',#14040,#11132,#11133);
#8935=AXIS2_PLACEMENT_3D('',#14041,#11134,#11135);
#8936=AXIS2_PLACEMENT_3D('',#14042,#11136,#11137);
#8937=AXIS2_PLACEMENT_3D('',#14043,#11138,#11139);
#8938=AXIS2_PLACEMENT_3D('',#14044,#11140,#11141);
#8939=AXIS2_PLACEMENT_3D('',#14045,#11142,#11143);
#8940=AXIS2_PLACEMENT_3D('',#14046,#11144,#11145);
#8941=AXIS2_PLACEMENT_3D('',#14047,#11146,#11147);
#8942=AXIS2_PLACEMENT_3D('',#14048,#11148,#11149);
#8943=AXIS2_PLACEMENT_3D('',#14049,#11150,#11151);
#8944=AXIS2_PLACEMENT_3D('',#14050,#11152,#11153);
#8945=AXIS2_PLACEMENT_3D('',#14051,#11154,#11155);
#8946=AXIS2_PLACEMENT_3D('',#14052,#11156,#11157);
#8947=AXIS2_PLACEMENT_3D('',#14053,#11158,#11159);
#8948=AXIS2_PLACEMENT_3D('',#14054,#11160,#11161);
#8949=AXIS2_PLACEMENT_3D('',#14055,#11162,#11163);
#8950=AXIS2_PLACEMENT_3D('',#14056,#11164,#11165);
#8951=AXIS2_PLACEMENT_3D('',#14057,#11166,#11167);
#8952=AXIS2_PLACEMENT_3D('',#14058,#11168,#11169);
#8953=AXIS2_PLACEMENT_3D('',#14059,#11170,#11171);
#8954=AXIS2_PLACEMENT_3D('',#14060,#11172,#11173);
#8955=AXIS2_PLACEMENT_3D('',#14061,#11174,#11175);
#8956=AXIS2_PLACEMENT_3D('',#14062,#11176,#11177);
#8957=AXIS2_PLACEMENT_3D('',#14063,#11178,#11179);
#8958=AXIS2_PLACEMENT_3D('',#14064,#11180,#11181);
#8959=AXIS2_PLACEMENT_3D('',#14065,#11182,#11183);
#8960=AXIS2_PLACEMENT_3D('',#14066,#11184,#11185);
#8961=AXIS2_PLACEMENT_3D('',#14067,#11186,#11187);
#8962=AXIS2_PLACEMENT_3D('',#14068,#11188,#11189);
#8963=AXIS2_PLACEMENT_3D('',#14069,#11190,#11191);
#8964=AXIS2_PLACEMENT_3D('',#14070,#11192,#11193);
#8965=AXIS2_PLACEMENT_3D('',#14071,#11194,#11195);
#8966=AXIS2_PLACEMENT_3D('',#14072,#11196,#11197);
#8967=AXIS2_PLACEMENT_3D('',#14073,#11198,#11199);
#8968=AXIS2_PLACEMENT_3D('',#14074,#11200,#11201);
#8969=AXIS2_PLACEMENT_3D('',#14075,#11202,#11203);
#8970=AXIS2_PLACEMENT_3D('',#14076,#11204,#11205);
#8971=AXIS2_PLACEMENT_3D('',#14077,#11206,#11207);
#8972=AXIS2_PLACEMENT_3D('',#14078,#11208,#11209);
#8973=AXIS2_PLACEMENT_3D('',#14079,#11210,#11211);
#8974=AXIS2_PLACEMENT_3D('',#14080,#11212,#11213);
#8975=AXIS2_PLACEMENT_3D('',#14081,#11214,#11215);
#8976=AXIS2_PLACEMENT_3D('',#14082,#11216,#11217);
#8977=AXIS2_PLACEMENT_3D('',#14083,#11218,#11219);
#8978=AXIS2_PLACEMENT_3D('',#14084,#11220,#11221);
#8979=AXIS2_PLACEMENT_3D('',#14085,#11222,#11223);
#8980=AXIS2_PLACEMENT_3D('',#14086,#11224,#11225);
#8981=AXIS2_PLACEMENT_3D('',#14087,#11226,#11227);
#8982=AXIS2_PLACEMENT_3D('',#14088,#11228,#11229);
#8983=AXIS2_PLACEMENT_3D('',#14089,#11230,#11231);
#8984=AXIS2_PLACEMENT_3D('',#14090,#11232,#11233);
#8985=AXIS2_PLACEMENT_3D('',#14091,#11234,#11235);
#8986=AXIS2_PLACEMENT_3D('',#14092,#11236,#11237);
#8987=AXIS2_PLACEMENT_3D('',#14093,#11238,#11239);
#8988=AXIS2_PLACEMENT_3D('',#14094,#11240,#11241);
#8989=AXIS2_PLACEMENT_3D('',#14095,#11242,#11243);
#8990=AXIS2_PLACEMENT_3D('',#14096,#11244,#11245);
#8991=AXIS2_PLACEMENT_3D('',#14097,#11246,#11247);
#8992=AXIS2_PLACEMENT_3D('',#14098,#11248,#11249);
#8993=AXIS2_PLACEMENT_3D('',#14100,#11250,#11251);
#8994=AXIS2_PLACEMENT_3D('',#14103,#11253,#11254);
#8995=AXIS2_PLACEMENT_3D('',#14104,#11255,#11256);
#8996=AXIS2_PLACEMENT_3D('',#14105,#11257,#11258);
#8997=AXIS2_PLACEMENT_3D('',#14107,#11259,#11260);
#8998=AXIS2_PLACEMENT_3D('',#14110,#11262,#11263);
#8999=AXIS2_PLACEMENT_3D('',#14111,#11264,#11265);
#9000=AXIS2_PLACEMENT_3D('',#14112,#11266,#11267);
#9001=AXIS2_PLACEMENT_3D('',#14114,#11268,#11269);
#9002=AXIS2_PLACEMENT_3D('',#14117,#11271,#11272);
#9003=AXIS2_PLACEMENT_3D('',#14118,#11273,#11274);
#9004=AXIS2_PLACEMENT_3D('',#14119,#11275,#11276);
#9005=AXIS2_PLACEMENT_3D('',#14120,#11277,#11278);
#9006=AXIS2_PLACEMENT_3D('',#14121,#11279,#11280);
#9007=AXIS2_PLACEMENT_3D('',#14123,#11281,#11282);
#9008=AXIS2_PLACEMENT_3D('',#14126,#11284,#11285);
#9009=AXIS2_PLACEMENT_3D('',#14127,#11286,#11287);
#9010=AXIS2_PLACEMENT_3D('',#14129,#11288,#11289);
#9011=AXIS2_PLACEMENT_3D('',#14132,#11291,#11292);
#9012=AXIS2_PLACEMENT_3D('',#14133,#11293,#11294);
#9013=AXIS2_PLACEMENT_3D('',#14134,#11295,#11296);
#9014=AXIS2_PLACEMENT_3D('',#14135,#11297,#11298);
#9015=AXIS2_PLACEMENT_3D('',#14136,#11299,#11300);
#9016=AXIS2_PLACEMENT_3D('',#14138,#11301,#11302);
#9017=AXIS2_PLACEMENT_3D('',#14141,#11304,#11305);
#9018=AXIS2_PLACEMENT_3D('',#14142,#11306,#11307);
#9019=AXIS2_PLACEMENT_3D('',#14144,#11308,#11309);
#9020=AXIS2_PLACEMENT_3D('',#14147,#11311,#11312);
#9021=AXIS2_PLACEMENT_3D('',#14148,#11313,#11314);
#9022=AXIS2_PLACEMENT_3D('',#14149,#11315,#11316);
#9023=AXIS2_PLACEMENT_3D('',#14150,#11317,#11318);
#9024=AXIS2_PLACEMENT_3D('',#14151,#11319,#11320);
#9025=AXIS2_PLACEMENT_3D('',#14155,#11322,#11323);
#9026=AXIS2_PLACEMENT_3D('',#14156,#11324,#11325);
#9027=AXIS2_PLACEMENT_3D('',#14169,#11326,#11327);
#9028=AXIS2_PLACEMENT_3D('',#14210,#11329,#11330);
#9029=AXIS2_PLACEMENT_3D('',#14221,#11331,#11332);
#9030=AXIS2_PLACEMENT_3D('',#14223,#11334,#11335);
#9031=AXIS2_PLACEMENT_3D('',#14225,#11336,#11337);
#9032=AXIS2_PLACEMENT_3D('',#14228,#11339,#11340);
#9033=AXIS2_PLACEMENT_3D('',#14229,#11341,#11342);
#9034=AXIS2_PLACEMENT_3D('',#14231,#11343,#11344);
#9035=AXIS2_PLACEMENT_3D('',#14234,#11346,#11347);
#9036=AXIS2_PLACEMENT_3D('',#14235,#11348,#11349);
#9037=AXIS2_PLACEMENT_3D('',#14236,#11350,#11351);
#9038=AXIS2_PLACEMENT_3D('',#14237,#11352,#11353);
#9039=AXIS2_PLACEMENT_3D('',#14238,#11354,#11355);
#9040=AXIS2_PLACEMENT_3D('',#14242,#11357,#11358);
#9041=AXIS2_PLACEMENT_3D('',#14243,#11359,#11360);
#9042=AXIS2_PLACEMENT_3D('',#14256,#11361,#11362);
#9043=AXIS2_PLACEMENT_3D('',#14297,#11364,#11365);
#9044=AXIS2_PLACEMENT_3D('',#14308,#11366,#11367);
#9045=AXIS2_PLACEMENT_3D('',#14310,#11369,#11370);
#9046=AXIS2_PLACEMENT_3D('',#14312,#11371,#11372);
#9047=AXIS2_PLACEMENT_3D('',#14315,#11374,#11375);
#9048=AXIS2_PLACEMENT_3D('',#14316,#11376,#11377);
#9049=AXIS2_PLACEMENT_3D('',#14318,#11378,#11379);
#9050=AXIS2_PLACEMENT_3D('',#14321,#11381,#11382);
#9051=AXIS2_PLACEMENT_3D('',#14322,#11383,#11384);
#9052=AXIS2_PLACEMENT_3D('',#14323,#11385,#11386);
#9053=AXIS2_PLACEMENT_3D('',#14324,#11387,#11388);
#9054=AXIS2_PLACEMENT_3D('',#14325,#11389,#11390);
#9055=AXIS2_PLACEMENT_3D('',#14327,#11391,#11392);
#9056=AXIS2_PLACEMENT_3D('',#14330,#11394,#11395);
#9057=AXIS2_PLACEMENT_3D('',#14331,#11396,#11397);
#9058=AXIS2_PLACEMENT_3D('',#14333,#11398,#11399);
#9059=AXIS2_PLACEMENT_3D('',#14336,#11401,#11402);
#9060=AXIS2_PLACEMENT_3D('',#14337,#11403,#11404);
#9061=AXIS2_PLACEMENT_3D('',#14338,#11405,#11406);
#9062=AXIS2_PLACEMENT_3D('',#14339,#11407,#11408);
#9063=AXIS2_PLACEMENT_3D('',#14340,#11409,#11410);
#9064=AXIS2_PLACEMENT_3D('',#14342,#11411,#11412);
#9065=AXIS2_PLACEMENT_3D('',#14345,#11414,#11415);
#9066=AXIS2_PLACEMENT_3D('',#14346,#11416,#11417);
#9067=AXIS2_PLACEMENT_3D('',#14348,#11418,#11419);
#9068=AXIS2_PLACEMENT_3D('',#14351,#11421,#11422);
#9069=AXIS2_PLACEMENT_3D('',#14352,#11423,#11424);
#9070=AXIS2_PLACEMENT_3D('',#14353,#11425,#11426);
#9071=AXIS2_PLACEMENT_3D('',#14354,#11427,#11428);
#9072=AXIS2_PLACEMENT_3D('',#14355,#11429,#11430);
#9073=AXIS2_PLACEMENT_3D('',#14359,#11432,#11433);
#9074=AXIS2_PLACEMENT_3D('',#14360,#11434,#11435);
#9075=AXIS2_PLACEMENT_3D('',#14377,#11436,#11437);
#9076=AXIS2_PLACEMENT_3D('',#14418,#11439,#11440);
#9077=AXIS2_PLACEMENT_3D('',#14433,#11441,#11442);
#9078=AXIS2_PLACEMENT_3D('',#14435,#11444,#11445);
#9079=AXIS2_PLACEMENT_3D('',#14437,#11446,#11447);
#9080=AXIS2_PLACEMENT_3D('',#14440,#11449,#11450);
#9081=AXIS2_PLACEMENT_3D('',#14441,#11451,#11452);
#9082=AXIS2_PLACEMENT_3D('',#14443,#11453,#11454);
#9083=AXIS2_PLACEMENT_3D('',#14446,#11456,#11457);
#9084=AXIS2_PLACEMENT_3D('',#14447,#11458,#11459);
#9085=AXIS2_PLACEMENT_3D('',#14448,#11460,#11461);
#9086=AXIS2_PLACEMENT_3D('',#14449,#11462,#11463);
#9087=AXIS2_PLACEMENT_3D('',#14450,#11464,#11465);
#9088=AXIS2_PLACEMENT_3D('',#14454,#11467,#11468);
#9089=AXIS2_PLACEMENT_3D('',#14455,#11469,#11470);
#9090=AXIS2_PLACEMENT_3D('',#14472,#11471,#11472);
#9091=AXIS2_PLACEMENT_3D('',#14513,#11474,#11475);
#9092=AXIS2_PLACEMENT_3D('',#14528,#11476,#11477);
#9093=AXIS2_PLACEMENT_3D('',#14530,#11479,#11480);
#9094=AXIS2_PLACEMENT_3D('',#14532,#11481,#11482);
#9095=AXIS2_PLACEMENT_3D('',#14535,#11484,#11485);
#9096=AXIS2_PLACEMENT_3D('',#14536,#11486,#11487);
#9097=AXIS2_PLACEMENT_3D('',#14538,#11488,#11489);
#9098=AXIS2_PLACEMENT_3D('',#14541,#11491,#11492);
#9099=AXIS2_PLACEMENT_3D('',#14542,#11493,#11494);
#9100=AXIS2_PLACEMENT_3D('',#14543,#11495,#11496);
#9101=AXIS2_PLACEMENT_3D('',#14544,#11497,#11498);
#9102=AXIS2_PLACEMENT_3D('',#14545,#11499,#11500);
#9103=AXIS2_PLACEMENT_3D('',#14549,#11502,#11503);
#9104=AXIS2_PLACEMENT_3D('',#14550,#11504,#11505);
#9105=AXIS2_PLACEMENT_3D('',#14563,#11506,#11507);
#9106=AXIS2_PLACEMENT_3D('',#14604,#11509,#11510);
#9107=AXIS2_PLACEMENT_3D('',#14615,#11511,#11512);
#9108=AXIS2_PLACEMENT_3D('',#14617,#11514,#11515);
#9109=AXIS2_PLACEMENT_3D('',#14619,#11516,#11517);
#9110=AXIS2_PLACEMENT_3D('',#14622,#11519,#11520);
#9111=AXIS2_PLACEMENT_3D('',#14623,#11521,#11522);
#9112=AXIS2_PLACEMENT_3D('',#14625,#11523,#11524);
#9113=AXIS2_PLACEMENT_3D('',#14628,#11526,#11527);
#9114=AXIS2_PLACEMENT_3D('',#14629,#11528,#11529);
#9115=AXIS2_PLACEMENT_3D('',#14631,#11530,#11531);
#9116=AXIS2_PLACEMENT_3D('',#14634,#11533,#11534);
#9117=AXIS2_PLACEMENT_3D('',#14635,#11535,#11536);
#9118=AXIS2_PLACEMENT_3D('',#14637,#11537,#11538);
#9119=AXIS2_PLACEMENT_3D('',#14640,#11540,#11541);
#9120=AXIS2_PLACEMENT_3D('',#14641,#11542,#11543);
#9121=AXIS2_PLACEMENT_3D('',#14643,#11544,#11545);
#9122=AXIS2_PLACEMENT_3D('',#14645,#11546,#11547);
#9123=AXIS2_PLACEMENT_3D('',#14646,#11548,#11549);
#9124=AXIS2_PLACEMENT_3D('',#14649,#11551,#11552);
#9125=AXIS2_PLACEMENT_3D('',#14650,#11553,#11554);
#9126=AXIS2_PLACEMENT_3D('',#14652,#11555,#11556);
#9127=AXIS2_PLACEMENT_3D('',#14655,#11558,#11559);
#9128=AXIS2_PLACEMENT_3D('',#14656,#11560,#11561);
#9129=AXIS2_PLACEMENT_3D('',#14658,#11562,#11563);
#9130=AXIS2_PLACEMENT_3D('',#14660,#11565,#11566);
#9131=AXIS2_PLACEMENT_3D('',#14661,#11567,#11568);
#9132=AXIS2_PLACEMENT_3D('',#14662,#11569,#11570);
#9133=AXIS2_PLACEMENT_3D('',#14663,#11571,#11572);
#9134=AXIS2_PLACEMENT_3D('',#14672,#11577,#11578);
#9135=AXIS2_PLACEMENT_3D('',#14678,#11582,#11583);
#9136=AXIS2_PLACEMENT_3D('',#14684,#11587,#11588);
#9137=AXIS2_PLACEMENT_3D('',#14690,#11592,#11593);
#9138=AXIS2_PLACEMENT_3D('',#14696,#11597,#11598);
#9139=AXIS2_PLACEMENT_3D('',#14699,#11601,#11602);
#9140=AXIS2_PLACEMENT_3D('',#14700,#11603,#11604);
#9141=AXIS2_PLACEMENT_3D('',#14702,#11605,#11606);
#9142=AXIS2_PLACEMENT_3D('',#14703,#11607,#11608);
#9143=AXIS2_PLACEMENT_3D('',#14705,#11609,#11610);
#9144=AXIS2_PLACEMENT_3D('',#14707,#11612,#11613);
#9145=AXIS2_PLACEMENT_3D('',#14709,#11614,#11615);
#9146=AXIS2_PLACEMENT_3D('',#14711,#11617,#11618);
#9147=AXIS2_PLACEMENT_3D('',#14713,#11619,#11620);
#9148=AXIS2_PLACEMENT_3D('',#14715,#11622,#11623);
#9149=AXIS2_PLACEMENT_3D('',#14716,#11624,#11625);
#9150=AXIS2_PLACEMENT_3D('',#14717,#11626,#11627);
#9151=AXIS2_PLACEMENT_3D('',#14718,#11628,#11629);
#9152=AXIS2_PLACEMENT_3D('',#14719,#11630,#11631);
#9153=AXIS2_PLACEMENT_3D('',#14720,#11632,#11633);
#9154=AXIS2_PLACEMENT_3D('',#14721,#11634,#11635);
#9155=AXIS2_PLACEMENT_3D('',#14722,#11636,#11637);
#9156=AXIS2_PLACEMENT_3D('',#14723,#11638,#11639);
#9157=AXIS2_PLACEMENT_3D('',#14724,#11640,#11641);
#9158=AXIS2_PLACEMENT_3D('',#14725,#11642,#11643);
#9159=AXIS2_PLACEMENT_3D('',#14726,#11644,#11645);
#9160=AXIS2_PLACEMENT_3D('',#14727,#11646,#11647);
#9161=AXIS2_PLACEMENT_3D('',#14728,#11648,#11649);
#9162=AXIS2_PLACEMENT_3D('',#14729,#11650,#11651);
#9163=AXIS2_PLACEMENT_3D('',#14730,#11652,#11653);
#9164=AXIS2_PLACEMENT_3D('',#14731,#11654,#11655);
#9165=AXIS2_PLACEMENT_3D('',#14732,#11656,#11657);
#9166=DIRECTION('axis',(0.,0.,1.));
#9167=DIRECTION('refdir',(1.,0.,0.));
#9168=DIRECTION('axis',(0.,0.,1.));
#9169=DIRECTION('refdir',(1.,0.,0.));
#9170=DIRECTION('axis',(0.,0.,1.));
#9171=DIRECTION('refdir',(1.,0.,0.));
#9172=DIRECTION('center_axis',(0.,0.,1.));
#9173=DIRECTION('ref_axis',(1.,0.,0.));
#9174=DIRECTION('center_axis',(0.,0.,1.));
#9175=DIRECTION('ref_axis',(1.,0.,0.));
#9176=DIRECTION('',(0.,0.,1.));
#9177=DIRECTION('center_axis',(0.,0.,-1.));
#9178=DIRECTION('ref_axis',(1.,0.,0.));
#9179=DIRECTION('center_axis',(0.,0.,1.));
#9180=DIRECTION('ref_axis',(1.,0.,0.));
#9181=DIRECTION('center_axis',(0.,0.,1.));
#9182=DIRECTION('ref_axis',(1.,0.,0.));
#9183=DIRECTION('',(0.,0.,1.));
#9184=DIRECTION('center_axis',(0.,0.,-1.));
#9185=DIRECTION('ref_axis',(1.,0.,0.));
#9186=DIRECTION('center_axis',(0.,0.,1.));
#9187=DIRECTION('ref_axis',(1.,0.,0.));
#9188=DIRECTION('center_axis',(0.,0.,1.));
#9189=DIRECTION('ref_axis',(1.,0.,0.));
#9190=DIRECTION('',(0.,0.,1.));
#9191=DIRECTION('center_axis',(0.,0.,-1.));
#9192=DIRECTION('ref_axis',(1.,0.,0.));
#9193=DIRECTION('center_axis',(0.,0.,1.));
#9194=DIRECTION('ref_axis',(1.,0.,0.));
#9195=DIRECTION('center_axis',(0.,0.,1.));
#9196=DIRECTION('ref_axis',(1.,0.,0.));
#9197=DIRECTION('',(0.,0.,1.));
#9198=DIRECTION('center_axis',(0.,0.,-1.));
#9199=DIRECTION('ref_axis',(1.,0.,0.));
#9200=DIRECTION('center_axis',(0.,0.,1.));
#9201=DIRECTION('ref_axis',(1.,0.,0.));
#9202=DIRECTION('center_axis',(0.,0.,1.));
#9203=DIRECTION('ref_axis',(1.,0.,0.));
#9204=DIRECTION('',(0.,0.,1.));
#9205=DIRECTION('center_axis',(0.,0.,-1.));
#9206=DIRECTION('ref_axis',(1.,0.,0.));
#9207=DIRECTION('center_axis',(0.,0.,1.));
#9208=DIRECTION('ref_axis',(1.,0.,0.));
#9209=DIRECTION('center_axis',(0.,0.,1.));
#9210=DIRECTION('ref_axis',(1.,0.,0.));
#9211=DIRECTION('',(0.,0.,1.));
#9212=DIRECTION('center_axis',(0.,0.,-1.));
#9213=DIRECTION('ref_axis',(1.,0.,0.));
#9214=DIRECTION('center_axis',(0.,0.,1.));
#9215=DIRECTION('ref_axis',(1.,0.,0.));
#9216=DIRECTION('center_axis',(0.,0.,1.));
#9217=DIRECTION('ref_axis',(1.,0.,0.));
#9218=DIRECTION('',(0.,0.,1.));
#9219=DIRECTION('center_axis',(0.,0.,-1.));
#9220=DIRECTION('ref_axis',(1.,0.,0.));
#9221=DIRECTION('center_axis',(0.,0.,1.));
#9222=DIRECTION('ref_axis',(1.,0.,0.));
#9223=DIRECTION('center_axis',(0.,0.,1.));
#9224=DIRECTION('ref_axis',(1.,0.,0.));
#9225=DIRECTION('',(0.,0.,1.));
#9226=DIRECTION('center_axis',(0.,0.,-1.));
#9227=DIRECTION('ref_axis',(1.,0.,0.));
#9228=DIRECTION('center_axis',(0.,0.,1.));
#9229=DIRECTION('ref_axis',(1.,0.,0.));
#9230=DIRECTION('center_axis',(0.,0.,1.));
#9231=DIRECTION('ref_axis',(1.,0.,0.));
#9232=DIRECTION('',(0.,0.,1.));
#9233=DIRECTION('center_axis',(0.,0.,-1.));
#9234=DIRECTION('ref_axis',(1.,0.,0.));
#9235=DIRECTION('center_axis',(0.,0.,1.));
#9236=DIRECTION('ref_axis',(1.,0.,0.));
#9237=DIRECTION('center_axis',(0.,0.,1.));
#9238=DIRECTION('ref_axis',(1.,0.,0.));
#9239=DIRECTION('',(0.,0.,1.));
#9240=DIRECTION('center_axis',(0.,0.,-1.));
#9241=DIRECTION('ref_axis',(1.,0.,0.));
#9242=DIRECTION('center_axis',(0.,0.,1.));
#9243=DIRECTION('ref_axis',(1.,0.,0.));
#9244=DIRECTION('center_axis',(0.,0.,1.));
#9245=DIRECTION('ref_axis',(1.,0.,0.));
#9246=DIRECTION('',(0.,0.,1.));
#9247=DIRECTION('center_axis',(0.,0.,-1.));
#9248=DIRECTION('ref_axis',(1.,0.,0.));
#9249=DIRECTION('center_axis',(0.,0.,1.));
#9250=DIRECTION('ref_axis',(1.,0.,0.));
#9251=DIRECTION('center_axis',(0.,0.,1.));
#9252=DIRECTION('ref_axis',(1.,0.,0.));
#9253=DIRECTION('',(0.,0.,1.));
#9254=DIRECTION('center_axis',(0.,0.,-1.));
#9255=DIRECTION('ref_axis',(1.,0.,0.));
#9256=DIRECTION('center_axis',(0.,1.,0.));
#9257=DIRECTION('ref_axis',(-1.,0.,0.));
#9258=DIRECTION('',(-1.,0.,0.));
#9259=DIRECTION('',(0.,0.,1.));
#9260=DIRECTION('',(-1.,0.,0.));
#9261=DIRECTION('',(0.,0.,1.));
#9262=DIRECTION('center_axis',(1.,0.,0.));
#9263=DIRECTION('ref_axis',(0.,1.,0.));
#9264=DIRECTION('',(0.,1.,0.));
#9265=DIRECTION('',(0.,1.,0.));
#9266=DIRECTION('',(0.,0.,1.));
#9267=DIRECTION('center_axis',(0.,-1.,0.));
#9268=DIRECTION('ref_axis',(1.,0.,0.));
#9269=DIRECTION('',(1.,0.,0.));
#9270=DIRECTION('',(1.,0.,0.));
#9271=DIRECTION('',(0.,0.,1.));
#9272=DIRECTION('center_axis',(-1.,0.,0.));
#9273=DIRECTION('ref_axis',(0.,-1.,0.));
#9274=DIRECTION('',(0.,-1.,0.));
#9275=DIRECTION('',(0.,-1.,0.));
#9276=DIRECTION('center_axis',(0.,0.,1.));
#9277=DIRECTION('ref_axis',(1.,0.,0.));
#9278=DIRECTION('center_axis',(0.,0.,1.));
#9279=DIRECTION('ref_axis',(1.,0.,0.));
#9280=DIRECTION('axis',(0.,0.,1.));
#9281=DIRECTION('refdir',(1.,0.,0.));
#9282=DIRECTION('center_axis',(0.,1.,0.));
#9283=DIRECTION('ref_axis',(1.,0.,0.));
#9284=DIRECTION('center_axis',(0.,1.,0.));
#9285=DIRECTION('ref_axis',(1.,0.,0.));
#9286=DIRECTION('',(0.,1.,0.));
#9287=DIRECTION('center_axis',(0.,-1.,0.));
#9288=DIRECTION('ref_axis',(1.,0.,0.));
#9289=DIRECTION('center_axis',(0.,1.,0.));
#9290=DIRECTION('ref_axis',(1.,0.,0.));
#9291=DIRECTION('center_axis',(0.,1.,0.));
#9292=DIRECTION('ref_axis',(1.,0.,0.));
#9293=DIRECTION('',(0.,1.,0.));
#9294=DIRECTION('center_axis',(0.,-1.,0.));
#9295=DIRECTION('ref_axis',(1.,0.,0.));
#9296=DIRECTION('center_axis',(0.,1.,0.));
#9297=DIRECTION('ref_axis',(1.,0.,0.));
#9298=DIRECTION('center_axis',(0.,1.,0.));
#9299=DIRECTION('ref_axis',(1.,0.,0.));
#9300=DIRECTION('',(0.,1.,0.));
#9301=DIRECTION('center_axis',(0.,-1.,0.));
#9302=DIRECTION('ref_axis',(1.,0.,0.));
#9303=DIRECTION('center_axis',(0.,1.,0.));
#9304=DIRECTION('ref_axis',(1.,0.,0.));
#9305=DIRECTION('center_axis',(0.,1.,0.));
#9306=DIRECTION('ref_axis',(1.,0.,0.));
#9307=DIRECTION('',(0.,1.,0.));
#9308=DIRECTION('center_axis',(0.,-1.,0.));
#9309=DIRECTION('ref_axis',(1.,0.,0.));
#9310=DIRECTION('center_axis',(0.,0.,1.));
#9311=DIRECTION('ref_axis',(1.,0.,0.));
#9312=DIRECTION('',(0.,-1.,0.));
#9313=DIRECTION('center_axis',(0.,0.,1.));
#9314=DIRECTION('ref_axis',(1.,0.,0.));
#9315=DIRECTION('center_axis',(0.,0.,1.));
#9316=DIRECTION('ref_axis',(1.,0.,0.));
#9317=DIRECTION('center_axis',(0.,0.,1.));
#9318=DIRECTION('ref_axis',(1.,0.,0.));
#9319=DIRECTION('',(0.,0.,1.));
#9320=DIRECTION('center_axis',(0.871575537124549,0.,-0.490261239632559));
#9321=DIRECTION('ref_axis',(0.490261239632559,0.,0.871575537124549));
#9322=DIRECTION('center_axis',(0.871575537124549,0.,-0.490261239632559));
#9323=DIRECTION('ref_axis',(0.490261239632559,0.,0.871575537124549));
#9324=DIRECTION('center_axis',(0.,0.,1.));
#9325=DIRECTION('ref_axis',(1.,0.,0.));
#9326=DIRECTION('center_axis',(0.,0.,1.));
#9327=DIRECTION('ref_axis',(1.,0.,0.));
#9328=DIRECTION('center_axis',(0.,0.,1.));
#9329=DIRECTION('ref_axis',(1.,0.,0.));
#9330=DIRECTION('',(0.,1.,0.));
#9331=DIRECTION('center_axis',(0.,0.,1.));
#9332=DIRECTION('ref_axis',(1.,0.,0.));
#9333=DIRECTION('center_axis',(0.,0.,1.));
#9334=DIRECTION('ref_axis',(1.,0.,0.));
#9335=DIRECTION('center_axis',(0.,0.,1.));
#9336=DIRECTION('ref_axis',(1.,0.,0.));
#9337=DIRECTION('center_axis',(0.,0.,1.));
#9338=DIRECTION('ref_axis',(1.,0.,0.));
#9339=DIRECTION('',(0.,0.,1.));
#9340=DIRECTION('center_axis',(-0.871575537124549,0.,-0.490261239632559));
#9341=DIRECTION('ref_axis',(0.490261239632559,0.,-0.871575537124549));
#9342=DIRECTION('center_axis',(0.,0.,1.));
#9343=DIRECTION('ref_axis',(1.,0.,0.));
#9344=DIRECTION('center_axis',(0.,0.,1.));
#9345=DIRECTION('ref_axis',(1.,0.,0.));
#9346=DIRECTION('center_axis',(0.,0.,1.));
#9347=DIRECTION('ref_axis',(1.,0.,0.));
#9348=DIRECTION('center_axis',(0.,0.,1.));
#9349=DIRECTION('ref_axis',(1.,0.,0.));
#9350=DIRECTION('',(0.,0.,1.));
#9351=DIRECTION('center_axis',(0.,0.,1.));
#9352=DIRECTION('ref_axis',(1.,0.,0.));
#9353=DIRECTION('center_axis',(0.,0.,1.));
#9354=DIRECTION('ref_axis',(1.,0.,0.));
#9355=DIRECTION('',(0.,0.,1.));
#9356=DIRECTION('center_axis',(0.871575537124549,0.,0.490261239632559));
#9357=DIRECTION('ref_axis',(0.490261239632559,0.,-0.871575537124549));
#9358=DIRECTION('',(0.,1.,0.));
#9359=DIRECTION('',(-0.490261239632559,0.,0.871575537124549));
#9360=DIRECTION('',(0.,1.,0.));
#9361=DIRECTION('',(0.490261239632559,0.,-0.871575537124549));
#9362=DIRECTION('center_axis',(-0.871575537124549,0.,0.490261239632559));
#9363=DIRECTION('ref_axis',(0.490261239632559,0.,0.871575537124549));
#9364=DIRECTION('',(0.,-1.,0.));
#9365=DIRECTION('',(0.490261239632559,0.,0.871575537124549));
#9366=DIRECTION('',(0.,1.,0.));
#9367=DIRECTION('',(-0.490261239632559,0.,-0.871575537124549));
#9368=DIRECTION('center_axis',(-1.,0.,0.));
#9369=DIRECTION('ref_axis',(0.,0.,1.));
#9370=DIRECTION('',(0.,0.,-1.));
#9371=DIRECTION('',(0.,0.,1.));
#9372=DIRECTION('',(0.,1.,0.));
#9373=DIRECTION('center_axis',(0.,0.,-1.));
#9374=DIRECTION('ref_axis',(-1.,0.,0.));
#9375=DIRECTION('',(1.,0.,0.));
#9376=DIRECTION('',(-1.,0.,0.));
#9377=DIRECTION('',(0.,1.,0.));
#9378=DIRECTION('center_axis',(1.,0.,0.));
#9379=DIRECTION('ref_axis',(0.,0.,-1.));
#9380=DIRECTION('',(0.,0.,1.));
#9381=DIRECTION('',(0.,0.,-1.));
#9382=DIRECTION('center_axis',(0.,1.,0.));
#9383=DIRECTION('ref_axis',(1.,0.,0.));
#9384=DIRECTION('center_axis',(0.,1.,0.));
#9385=DIRECTION('ref_axis',(1.,0.,0.));
#9386=DIRECTION('center_axis',(0.,-1.,0.));
#9387=DIRECTION('ref_axis',(1.,0.,0.));
#9388=DIRECTION('center_axis',(0.,1.,0.));
#9389=DIRECTION('ref_axis',(1.,0.,0.));
#9390=DIRECTION('',(0.,-1.,0.));
#9391=DIRECTION('center_axis',(0.,-1.,0.));
#9392=DIRECTION('ref_axis',(1.,0.,0.));
#9393=DIRECTION('center_axis',(0.,1.,0.));
#9394=DIRECTION('ref_axis',(6.12323399573677E-17,0.,1.));
#9395=DIRECTION('center_axis',(0.,1.,0.));
#9396=DIRECTION('ref_axis',(1.,0.,0.));
#9397=DIRECTION('center_axis',(0.,1.,0.));
#9398=DIRECTION('ref_axis',(1.,0.,0.));
#9399=DIRECTION('axis',(0.,0.,1.));
#9400=DIRECTION('refdir',(1.,0.,0.));
#9401=DIRECTION('center_axis',(0.,1.,0.));
#9402=DIRECTION('ref_axis',(1.,0.,0.));
#9403=DIRECTION('center_axis',(0.,1.,0.));
#9404=DIRECTION('ref_axis',(1.,0.,0.));
#9405=DIRECTION('',(0.,1.,0.));
#9406=DIRECTION('center_axis',(0.,-1.,0.));
#9407=DIRECTION('ref_axis',(1.,0.,0.));
#9408=DIRECTION('center_axis',(0.,1.,0.));
#9409=DIRECTION('ref_axis',(1.,0.,0.));
#9410=DIRECTION('center_axis',(0.,1.,0.));
#9411=DIRECTION('ref_axis',(1.,0.,0.));
#9412=DIRECTION('',(0.,1.,0.));
#9413=DIRECTION('center_axis',(0.,-1.,0.));
#9414=DIRECTION('ref_axis',(1.,0.,0.));
#9415=DIRECTION('center_axis',(0.,1.,0.));
#9416=DIRECTION('ref_axis',(1.,0.,0.));
#9417=DIRECTION('center_axis',(0.,1.,0.));
#9418=DIRECTION('ref_axis',(1.,0.,0.));
#9419=DIRECTION('',(0.,1.,0.));
#9420=DIRECTION('center_axis',(0.,-1.,0.));
#9421=DIRECTION('ref_axis',(1.,0.,0.));
#9422=DIRECTION('center_axis',(0.,1.,0.));
#9423=DIRECTION('ref_axis',(1.,0.,0.));
#9424=DIRECTION('center_axis',(0.,1.,0.));
#9425=DIRECTION('ref_axis',(1.,0.,0.));
#9426=DIRECTION('',(0.,1.,0.));
#9427=DIRECTION('center_axis',(0.,-1.,0.));
#9428=DIRECTION('ref_axis',(1.,0.,0.));
#9429=DIRECTION('center_axis',(0.,1.,0.));
#9430=DIRECTION('ref_axis',(1.,0.,0.));
#9431=DIRECTION('center_axis',(0.,1.,0.));
#9432=DIRECTION('ref_axis',(1.,0.,0.));
#9433=DIRECTION('',(0.,-1.,0.));
#9434=DIRECTION('center_axis',(0.,-1.,0.));
#9435=DIRECTION('ref_axis',(1.,0.,0.));
#9436=DIRECTION('center_axis',(0.,1.,0.));
#9437=DIRECTION('ref_axis',(1.,0.,0.));
#9438=DIRECTION('center_axis',(0.,-1.,0.));
#9439=DIRECTION('ref_axis',(1.,0.,0.));
#9440=DIRECTION('center_axis',(0.,1.,0.));
#9441=DIRECTION('ref_axis',(1.,0.,0.));
#9442=DIRECTION('',(0.,-1.,0.));
#9443=DIRECTION('center_axis',(0.,-1.,0.));
#9444=DIRECTION('ref_axis',(1.,0.,0.));
#9445=DIRECTION('center_axis',(0.,1.,0.));
#9446=DIRECTION('ref_axis',(1.,0.,0.));
#9447=DIRECTION('center_axis',(0.,1.,0.));
#9448=DIRECTION('ref_axis',(1.,0.,0.));
#9449=DIRECTION('',(0.,-1.,0.));
#9450=DIRECTION('center_axis',(0.,1.,0.));
#9451=DIRECTION('ref_axis',(1.,0.,0.));
#9452=DIRECTION('center_axis',(0.,1.,0.));
#9453=DIRECTION('ref_axis',(1.,0.,0.));
#9454=DIRECTION('center_axis',(0.,1.,0.));
#9455=DIRECTION('ref_axis',(1.,0.,0.));
#9456=DIRECTION('axis',(0.,0.,1.));
#9457=DIRECTION('refdir',(1.,0.,0.));
#9458=DIRECTION('center_axis',(0.,1.,0.));
#9459=DIRECTION('ref_axis',(1.,0.,0.));
#9460=DIRECTION('center_axis',(0.,1.,0.));
#9461=DIRECTION('ref_axis',(1.,0.,0.));
#9462=DIRECTION('',(0.,1.,0.));
#9463=DIRECTION('center_axis',(0.,-1.,0.));
#9464=DIRECTION('ref_axis',(1.,0.,0.));
#9465=DIRECTION('center_axis',(0.,1.,0.));
#9466=DIRECTION('ref_axis',(1.,0.,0.));
#9467=DIRECTION('center_axis',(0.,1.,0.));
#9468=DIRECTION('ref_axis',(1.,0.,0.));
#9469=DIRECTION('',(0.,1.,0.));
#9470=DIRECTION('center_axis',(0.,-1.,0.));
#9471=DIRECTION('ref_axis',(1.,0.,0.));
#9472=DIRECTION('center_axis',(0.,1.,0.));
#9473=DIRECTION('ref_axis',(1.,0.,0.));
#9474=DIRECTION('center_axis',(0.,1.,0.));
#9475=DIRECTION('ref_axis',(1.,0.,0.));
#9476=DIRECTION('',(0.,1.,0.));
#9477=DIRECTION('center_axis',(0.,-1.,0.));
#9478=DIRECTION('ref_axis',(1.,0.,0.));
#9479=DIRECTION('center_axis',(0.,1.,0.));
#9480=DIRECTION('ref_axis',(1.,0.,0.));
#9481=DIRECTION('center_axis',(0.,1.,0.));
#9482=DIRECTION('ref_axis',(1.,0.,0.));
#9483=DIRECTION('',(0.,1.,0.));
#9484=DIRECTION('center_axis',(0.,-1.,0.));
#9485=DIRECTION('ref_axis',(1.,0.,0.));
#9486=DIRECTION('center_axis',(0.,1.,0.));
#9487=DIRECTION('ref_axis',(1.,0.,0.));
#9488=DIRECTION('center_axis',(0.,1.,0.));
#9489=DIRECTION('ref_axis',(1.,0.,0.));
#9490=DIRECTION('',(0.,-1.,0.));
#9491=DIRECTION('center_axis',(0.,1.,0.));
#9492=DIRECTION('ref_axis',(1.,0.,0.));
#9493=DIRECTION('center_axis',(0.,1.,0.));
#9494=DIRECTION('ref_axis',(1.,0.,0.));
#9495=DIRECTION('center_axis',(0.,-1.,0.));
#9496=DIRECTION('ref_axis',(1.,0.,0.));
#9497=DIRECTION('center_axis',(0.,1.,0.));
#9498=DIRECTION('ref_axis',(1.,0.,0.));
#9499=DIRECTION('center_axis',(0.,-1.,0.));
#9500=DIRECTION('ref_axis',(1.,0.,0.));
#9501=DIRECTION('',(0.,-1.,0.));
#9502=DIRECTION('center_axis',(0.,1.,0.));
#9503=DIRECTION('ref_axis',(1.,0.,0.));
#9504=DIRECTION('center_axis',(0.,1.,0.));
#9505=DIRECTION('ref_axis',(1.,0.,0.));
#9506=DIRECTION('',(0.,-1.,0.));
#9507=DIRECTION('center_axis',(0.,1.,0.));
#9508=DIRECTION('ref_axis',(1.,0.,0.));
#9509=DIRECTION('center_axis',(0.,1.,0.));
#9510=DIRECTION('ref_axis',(1.,0.,0.));
#9511=DIRECTION('center_axis',(0.,1.,0.));
#9512=DIRECTION('ref_axis',(1.,0.,0.));
#9513=DIRECTION('axis',(0.,0.,1.));
#9514=DIRECTION('refdir',(1.,0.,0.));
#9515=DIRECTION('center_axis',(0.,1.,0.));
#9516=DIRECTION('ref_axis',(1.,0.,0.));
#9517=DIRECTION('center_axis',(0.,1.,0.));
#9518=DIRECTION('ref_axis',(1.,0.,0.));
#9519=DIRECTION('',(0.,1.,0.));
#9520=DIRECTION('center_axis',(0.,-1.,0.));
#9521=DIRECTION('ref_axis',(1.,0.,0.));
#9522=DIRECTION('center_axis',(0.,1.,0.));
#9523=DIRECTION('ref_axis',(1.,0.,0.));
#9524=DIRECTION('center_axis',(0.,1.,0.));
#9525=DIRECTION('ref_axis',(1.,0.,0.));
#9526=DIRECTION('',(0.,1.,0.));
#9527=DIRECTION('center_axis',(0.,-1.,0.));
#9528=DIRECTION('ref_axis',(1.,0.,0.));
#9529=DIRECTION('center_axis',(0.,1.,0.));
#9530=DIRECTION('ref_axis',(1.,0.,0.));
#9531=DIRECTION('center_axis',(0.,1.,0.));
#9532=DIRECTION('ref_axis',(1.,0.,0.));
#9533=DIRECTION('',(0.,1.,0.));
#9534=DIRECTION('center_axis',(0.,-1.,0.));
#9535=DIRECTION('ref_axis',(1.,0.,0.));
#9536=DIRECTION('center_axis',(0.,1.,0.));
#9537=DIRECTION('ref_axis',(1.,0.,0.));
#9538=DIRECTION('center_axis',(0.,1.,0.));
#9539=DIRECTION('ref_axis',(1.,0.,0.));
#9540=DIRECTION('',(0.,1.,0.));
#9541=DIRECTION('center_axis',(0.,-1.,0.));
#9542=DIRECTION('ref_axis',(1.,0.,0.));
#9543=DIRECTION('center_axis',(0.,0.,1.));
#9544=DIRECTION('ref_axis',(1.,0.,0.));
#9545=DIRECTION('',(0.,-1.,0.));
#9546=DIRECTION('center_axis',(0.,0.,1.));
#9547=DIRECTION('ref_axis',(1.,0.,0.));
#9548=DIRECTION('center_axis',(0.,0.,1.));
#9549=DIRECTION('ref_axis',(1.,0.,0.));
#9550=DIRECTION('center_axis',(0.,0.,1.));
#9551=DIRECTION('ref_axis',(1.,0.,0.));
#9552=DIRECTION('',(0.,0.,1.));
#9553=DIRECTION('center_axis',(0.871575537124549,0.,-0.490261239632559));
#9554=DIRECTION('ref_axis',(0.490261239632559,0.,0.871575537124549));
#9555=DIRECTION('center_axis',(0.871575537124549,0.,-0.490261239632559));
#9556=DIRECTION('ref_axis',(0.490261239632559,0.,0.871575537124549));
#9557=DIRECTION('center_axis',(0.,0.,1.));
#9558=DIRECTION('ref_axis',(1.,0.,0.));
#9559=DIRECTION('center_axis',(0.,0.,1.));
#9560=DIRECTION('ref_axis',(1.,0.,0.));
#9561=DIRECTION('center_axis',(0.,0.,1.));
#9562=DIRECTION('ref_axis',(1.,0.,0.));
#9563=DIRECTION('',(0.,1.,0.));
#9564=DIRECTION('center_axis',(0.,0.,1.));
#9565=DIRECTION('ref_axis',(1.,0.,0.));
#9566=DIRECTION('center_axis',(0.,0.,1.));
#9567=DIRECTION('ref_axis',(1.,0.,0.));
#9568=DIRECTION('center_axis',(0.,0.,1.));
#9569=DIRECTION('ref_axis',(1.,0.,0.));
#9570=DIRECTION('center_axis',(0.,0.,1.));
#9571=DIRECTION('ref_axis',(1.,0.,0.));
#9572=DIRECTION('',(0.,0.,1.));
#9573=DIRECTION('center_axis',(-0.871575537124549,0.,-0.490261239632559));
#9574=DIRECTION('ref_axis',(0.490261239632559,0.,-0.871575537124549));
#9575=DIRECTION('center_axis',(0.,0.,1.));
#9576=DIRECTION('ref_axis',(1.,0.,0.));
#9577=DIRECTION('center_axis',(0.,0.,1.));
#9578=DIRECTION('ref_axis',(1.,0.,0.));
#9579=DIRECTION('center_axis',(0.,0.,1.));
#9580=DIRECTION('ref_axis',(1.,0.,0.));
#9581=DIRECTION('center_axis',(0.,0.,1.));
#9582=DIRECTION('ref_axis',(1.,0.,0.));
#9583=DIRECTION('',(0.,0.,1.));
#9584=DIRECTION('center_axis',(0.,0.,1.));
#9585=DIRECTION('ref_axis',(1.,0.,0.));
#9586=DIRECTION('center_axis',(0.,0.,1.));
#9587=DIRECTION('ref_axis',(1.,0.,0.));
#9588=DIRECTION('',(0.,0.,1.));
#9589=DIRECTION('center_axis',(0.871575537124549,0.,0.490261239632559));
#9590=DIRECTION('ref_axis',(0.490261239632559,0.,-0.871575537124549));
#9591=DIRECTION('',(0.,1.,0.));
#9592=DIRECTION('',(-0.490261239632559,0.,0.871575537124549));
#9593=DIRECTION('',(0.,1.,0.));
#9594=DIRECTION('',(0.490261239632559,0.,-0.871575537124549));
#9595=DIRECTION('center_axis',(-0.871575537124549,0.,0.490261239632559));
#9596=DIRECTION('ref_axis',(0.490261239632559,0.,0.871575537124549));
#9597=DIRECTION('',(0.,-1.,0.));
#9598=DIRECTION('',(0.490261239632559,0.,0.871575537124549));
#9599=DIRECTION('',(0.,1.,0.));
#9600=DIRECTION('',(-0.490261239632559,0.,-0.871575537124549));
#9601=DIRECTION('center_axis',(-1.,0.,0.));
#9602=DIRECTION('ref_axis',(0.,0.,1.));
#9603=DIRECTION('',(0.,0.,-1.));
#9604=DIRECTION('',(0.,0.,1.));
#9605=DIRECTION('',(0.,1.,0.));
#9606=DIRECTION('center_axis',(0.,0.,-1.));
#9607=DIRECTION('ref_axis',(-1.,0.,0.));
#9608=DIRECTION('',(1.,0.,0.));
#9609=DIRECTION('',(-1.,0.,0.));
#9610=DIRECTION('',(0.,1.,0.));
#9611=DIRECTION('center_axis',(1.,0.,0.));
#9612=DIRECTION('ref_axis',(0.,0.,-1.));
#9613=DIRECTION('',(0.,0.,1.));
#9614=DIRECTION('',(0.,0.,-1.));
#9615=DIRECTION('center_axis',(0.,1.,0.));
#9616=DIRECTION('ref_axis',(1.,0.,0.));
#9617=DIRECTION('center_axis',(0.,1.,0.));
#9618=DIRECTION('ref_axis',(1.,0.,0.));
#9619=DIRECTION('center_axis',(0.,-1.,0.));
#9620=DIRECTION('ref_axis',(1.,0.,0.));
#9621=DIRECTION('center_axis',(0.,1.,0.));
#9622=DIRECTION('ref_axis',(1.,0.,0.));
#9623=DIRECTION('',(0.,-1.,0.));
#9624=DIRECTION('center_axis',(0.,-1.,0.));
#9625=DIRECTION('ref_axis',(1.,0.,0.));
#9626=DIRECTION('center_axis',(0.,1.,0.));
#9627=DIRECTION('ref_axis',(6.12323399573677E-17,0.,1.));
#9628=DIRECTION('center_axis',(0.,1.,0.));
#9629=DIRECTION('ref_axis',(1.,0.,0.));
#9630=DIRECTION('center_axis',(0.,1.,0.));
#9631=DIRECTION('ref_axis',(1.,0.,0.));
#9632=DIRECTION('axis',(0.,0.,1.));
#9633=DIRECTION('refdir',(1.,0.,0.));
#9634=DIRECTION('center_axis',(0.,1.,0.));
#9635=DIRECTION('ref_axis',(1.,0.,0.));
#9636=DIRECTION('center_axis',(0.,1.,0.));
#9637=DIRECTION('ref_axis',(1.,0.,0.));
#9638=DIRECTION('',(0.,1.,0.));
#9639=DIRECTION('center_axis',(0.,-1.,0.));
#9640=DIRECTION('ref_axis',(1.,0.,0.));
#9641=DIRECTION('center_axis',(0.,1.,0.));
#9642=DIRECTION('ref_axis',(1.,0.,0.));
#9643=DIRECTION('center_axis',(0.,1.,0.));
#9644=DIRECTION('ref_axis',(1.,0.,0.));
#9645=DIRECTION('',(0.,1.,0.));
#9646=DIRECTION('center_axis',(0.,-1.,0.));
#9647=DIRECTION('ref_axis',(1.,0.,0.));
#9648=DIRECTION('center_axis',(0.,1.,0.));
#9649=DIRECTION('ref_axis',(1.,0.,0.));
#9650=DIRECTION('center_axis',(0.,1.,0.));
#9651=DIRECTION('ref_axis',(1.,0.,0.));
#9652=DIRECTION('',(0.,1.,0.));
#9653=DIRECTION('center_axis',(0.,-1.,0.));
#9654=DIRECTION('ref_axis',(1.,0.,0.));
#9655=DIRECTION('center_axis',(0.,1.,0.));
#9656=DIRECTION('ref_axis',(1.,0.,0.));
#9657=DIRECTION('center_axis',(0.,1.,0.));
#9658=DIRECTION('ref_axis',(1.,0.,0.));
#9659=DIRECTION('',(0.,1.,0.));
#9660=DIRECTION('center_axis',(0.,-1.,0.));
#9661=DIRECTION('ref_axis',(1.,0.,0.));
#9662=DIRECTION('center_axis',(0.,1.,0.));
#9663=DIRECTION('ref_axis',(1.,0.,0.));
#9664=DIRECTION('center_axis',(0.,1.,0.));
#9665=DIRECTION('ref_axis',(1.,0.,0.));
#9666=DIRECTION('',(0.,-1.,0.));
#9667=DIRECTION('center_axis',(0.,-1.,0.));
#9668=DIRECTION('ref_axis',(1.,0.,0.));
#9669=DIRECTION('center_axis',(0.,1.,0.));
#9670=DIRECTION('ref_axis',(1.,0.,0.));
#9671=DIRECTION('center_axis',(0.,-1.,0.));
#9672=DIRECTION('ref_axis',(1.,0.,0.));
#9673=DIRECTION('center_axis',(0.,1.,0.));
#9674=DIRECTION('ref_axis',(1.,0.,0.));
#9675=DIRECTION('',(0.,-1.,0.));
#9676=DIRECTION('center_axis',(0.,-1.,0.));
#9677=DIRECTION('ref_axis',(1.,0.,0.));
#9678=DIRECTION('center_axis',(0.,1.,0.));
#9679=DIRECTION('ref_axis',(1.,0.,0.));
#9680=DIRECTION('center_axis',(0.,1.,0.));
#9681=DIRECTION('ref_axis',(1.,0.,0.));
#9682=DIRECTION('',(0.,-1.,0.));
#9683=DIRECTION('center_axis',(0.,1.,0.));
#9684=DIRECTION('ref_axis',(1.,0.,0.));
#9685=DIRECTION('center_axis',(0.,1.,0.));
#9686=DIRECTION('ref_axis',(1.,0.,0.));
#9687=DIRECTION('center_axis',(0.,1.,0.));
#9688=DIRECTION('ref_axis',(1.,0.,0.));
#9689=DIRECTION('axis',(0.,0.,1.));
#9690=DIRECTION('refdir',(1.,0.,0.));
#9691=DIRECTION('center_axis',(0.,1.,0.));
#9692=DIRECTION('ref_axis',(1.,0.,0.));
#9693=DIRECTION('center_axis',(0.,1.,0.));
#9694=DIRECTION('ref_axis',(1.,0.,0.));
#9695=DIRECTION('',(0.,1.,0.));
#9696=DIRECTION('center_axis',(0.,-1.,0.));
#9697=DIRECTION('ref_axis',(1.,0.,0.));
#9698=DIRECTION('center_axis',(0.,1.,0.));
#9699=DIRECTION('ref_axis',(1.,0.,0.));
#9700=DIRECTION('center_axis',(0.,1.,0.));
#9701=DIRECTION('ref_axis',(1.,0.,0.));
#9702=DIRECTION('',(0.,1.,0.));
#9703=DIRECTION('center_axis',(0.,-1.,0.));
#9704=DIRECTION('ref_axis',(1.,0.,0.));
#9705=DIRECTION('center_axis',(0.,1.,0.));
#9706=DIRECTION('ref_axis',(1.,0.,0.));
#9707=DIRECTION('center_axis',(0.,1.,0.));
#9708=DIRECTION('ref_axis',(1.,0.,0.));
#9709=DIRECTION('',(0.,1.,0.));
#9710=DIRECTION('center_axis',(0.,-1.,0.));
#9711=DIRECTION('ref_axis',(1.,0.,0.));
#9712=DIRECTION('center_axis',(0.,1.,0.));
#9713=DIRECTION('ref_axis',(1.,0.,0.));
#9714=DIRECTION('center_axis',(0.,1.,0.));
#9715=DIRECTION('ref_axis',(1.,0.,0.));
#9716=DIRECTION('',(0.,1.,0.));
#9717=DIRECTION('center_axis',(0.,-1.,0.));
#9718=DIRECTION('ref_axis',(1.,0.,0.));
#9719=DIRECTION('center_axis',(0.,1.,0.));
#9720=DIRECTION('ref_axis',(1.,0.,0.));
#9721=DIRECTION('center_axis',(0.,1.,0.));
#9722=DIRECTION('ref_axis',(1.,0.,0.));
#9723=DIRECTION('',(0.,-1.,0.));
#9724=DIRECTION('center_axis',(0.,1.,0.));
#9725=DIRECTION('ref_axis',(1.,0.,0.));
#9726=DIRECTION('center_axis',(0.,1.,0.));
#9727=DIRECTION('ref_axis',(1.,0.,0.));
#9728=DIRECTION('center_axis',(0.,-1.,0.));
#9729=DIRECTION('ref_axis',(1.,0.,0.));
#9730=DIRECTION('center_axis',(0.,1.,0.));
#9731=DIRECTION('ref_axis',(1.,0.,0.));
#9732=DIRECTION('center_axis',(0.,-1.,0.));
#9733=DIRECTION('ref_axis',(1.,0.,0.));
#9734=DIRECTION('',(0.,-1.,0.));
#9735=DIRECTION('center_axis',(0.,1.,0.));
#9736=DIRECTION('ref_axis',(1.,0.,0.));
#9737=DIRECTION('center_axis',(0.,1.,0.));
#9738=DIRECTION('ref_axis',(1.,0.,0.));
#9739=DIRECTION('',(0.,-1.,0.));
#9740=DIRECTION('center_axis',(0.,1.,0.));
#9741=DIRECTION('ref_axis',(1.,0.,0.));
#9742=DIRECTION('center_axis',(0.,1.,0.));
#9743=DIRECTION('ref_axis',(1.,0.,0.));
#9744=DIRECTION('center_axis',(0.,1.,0.));
#9745=DIRECTION('ref_axis',(1.,0.,0.));
#9746=DIRECTION('axis',(0.,0.,1.));
#9747=DIRECTION('refdir',(1.,0.,0.));
#9748=DIRECTION('center_axis',(0.,1.,0.));
#9749=DIRECTION('ref_axis',(1.,0.,0.));
#9750=DIRECTION('center_axis',(0.,1.,0.));
#9751=DIRECTION('ref_axis',(1.,0.,0.));
#9752=DIRECTION('',(0.,1.,0.));
#9753=DIRECTION('center_axis',(0.,-1.,0.));
#9754=DIRECTION('ref_axis',(1.,0.,0.));
#9755=DIRECTION('center_axis',(0.,1.,0.));
#9756=DIRECTION('ref_axis',(1.,0.,0.));
#9757=DIRECTION('center_axis',(0.,1.,0.));
#9758=DIRECTION('ref_axis',(1.,0.,0.));
#9759=DIRECTION('',(0.,1.,0.));
#9760=DIRECTION('center_axis',(0.,-1.,0.));
#9761=DIRECTION('ref_axis',(1.,0.,0.));
#9762=DIRECTION('center_axis',(0.,1.,0.));
#9763=DIRECTION('ref_axis',(1.,0.,0.));
#9764=DIRECTION('center_axis',(0.,1.,0.));
#9765=DIRECTION('ref_axis',(1.,0.,0.));
#9766=DIRECTION('',(0.,1.,0.));
#9767=DIRECTION('center_axis',(0.,-1.,0.));
#9768=DIRECTION('ref_axis',(1.,0.,0.));
#9769=DIRECTION('center_axis',(0.,1.,0.));
#9770=DIRECTION('ref_axis',(1.,0.,0.));
#9771=DIRECTION('center_axis',(0.,1.,0.));
#9772=DIRECTION('ref_axis',(1.,0.,0.));
#9773=DIRECTION('',(0.,1.,0.));
#9774=DIRECTION('center_axis',(0.,-1.,0.));
#9775=DIRECTION('ref_axis',(1.,0.,0.));
#9776=DIRECTION('center_axis',(0.,0.,-1.));
#9777=DIRECTION('ref_axis',(-1.,0.,0.));
#9778=DIRECTION('',(0.,-1.,0.));
#9779=DIRECTION('',(-1.,0.,0.));
#9780=DIRECTION('',(0.,1.,0.));
#9781=DIRECTION('',(1.,0.,0.));
#9782=DIRECTION('center_axis',(0.,1.,0.));
#9783=DIRECTION('ref_axis',(0.,0.,1.));
#9784=DIRECTION('center_axis',(0.,1.,0.));
#9785=DIRECTION('ref_axis',(1.,0.,0.));
#9786=DIRECTION('',(1.,0.,0.));
#9787=DIRECTION('',(0.,0.,-1.));
#9788=DIRECTION('center_axis',(0.,1.,0.));
#9789=DIRECTION('ref_axis',(1.,0.,0.));
#9790=DIRECTION('center_axis',(0.,-1.,0.));
#9791=DIRECTION('ref_axis',(1.,0.,0.));
#9792=DIRECTION('',(0.,0.,1.));
#9793=DIRECTION('',(-1.,0.,0.));
#9794=DIRECTION('center_axis',(0.,0.,1.));
#9795=DIRECTION('ref_axis',(1.,0.,0.));
#9796=DIRECTION('',(0.,1.,0.));
#9797=DIRECTION('',(0.,1.,0.));
#9798=DIRECTION('center_axis',(1.,0.,0.));
#9799=DIRECTION('ref_axis',(0.,0.,-1.));
#9800=DIRECTION('center_axis',(0.,1.,0.));
#9801=DIRECTION('ref_axis',(1.,0.,0.));
#9802=DIRECTION('center_axis',(0.,-1.,0.));
#9803=DIRECTION('ref_axis',(1.,0.,0.));
#9804=DIRECTION('',(0.,-1.,0.));
#9805=DIRECTION('center_axis',(0.,-1.,0.));
#9806=DIRECTION('ref_axis',(1.,0.,0.));
#9807=DIRECTION('center_axis',(0.,1.,0.));
#9808=DIRECTION('ref_axis',(1.,0.,0.));
#9809=DIRECTION('center_axis',(0.,1.,0.));
#9810=DIRECTION('ref_axis',(1.,0.,0.));
#9811=DIRECTION('',(0.,-1.,0.));
#9812=DIRECTION('center_axis',(0.,1.,0.));
#9813=DIRECTION('ref_axis',(1.,0.,0.));
#9814=DIRECTION('center_axis',(0.,1.,0.));
#9815=DIRECTION('ref_axis',(1.,0.,0.));
#9816=DIRECTION('center_axis',(0.,1.,0.));
#9817=DIRECTION('ref_axis',(1.,0.,0.));
#9818=DIRECTION('axis',(0.,0.,1.));
#9819=DIRECTION('refdir',(1.,0.,0.));
#9820=DIRECTION('center_axis',(0.,1.,0.));
#9821=DIRECTION('ref_axis',(1.,0.,0.));
#9822=DIRECTION('center_axis',(0.,1.,0.));
#9823=DIRECTION('ref_axis',(1.,0.,0.));
#9824=DIRECTION('',(0.,1.,0.));
#9825=DIRECTION('center_axis',(0.,-1.,0.));
#9826=DIRECTION('ref_axis',(1.,0.,0.));
#9827=DIRECTION('center_axis',(0.,1.,0.));
#9828=DIRECTION('ref_axis',(1.,0.,0.));
#9829=DIRECTION('center_axis',(0.,1.,0.));
#9830=DIRECTION('ref_axis',(1.,0.,0.));
#9831=DIRECTION('',(0.,1.,0.));
#9832=DIRECTION('center_axis',(0.,-1.,0.));
#9833=DIRECTION('ref_axis',(1.,0.,0.));
#9834=DIRECTION('center_axis',(0.,1.,0.));
#9835=DIRECTION('ref_axis',(1.,0.,0.));
#9836=DIRECTION('center_axis',(0.,1.,0.));
#9837=DIRECTION('ref_axis',(1.,0.,0.));
#9838=DIRECTION('',(0.,1.,0.));
#9839=DIRECTION('center_axis',(0.,-1.,0.));
#9840=DIRECTION('ref_axis',(1.,0.,0.));
#9841=DIRECTION('center_axis',(0.,1.,0.));
#9842=DIRECTION('ref_axis',(1.,0.,0.));
#9843=DIRECTION('center_axis',(0.,1.,0.));
#9844=DIRECTION('ref_axis',(1.,0.,0.));
#9845=DIRECTION('',(0.,1.,0.));
#9846=DIRECTION('center_axis',(0.,-1.,0.));
#9847=DIRECTION('ref_axis',(1.,0.,0.));
#9848=DIRECTION('center_axis',(0.,1.,0.));
#9849=DIRECTION('ref_axis',(1.,0.,0.));
#9850=DIRECTION('center_axis',(0.,1.,0.));
#9851=DIRECTION('ref_axis',(1.,0.,0.));
#9852=DIRECTION('',(0.,-1.,0.));
#9853=DIRECTION('center_axis',(0.,-1.,0.));
#9854=DIRECTION('ref_axis',(1.,0.,0.));
#9855=DIRECTION('center_axis',(0.,1.,0.));
#9856=DIRECTION('ref_axis',(1.,0.,0.));
#9857=DIRECTION('center_axis',(0.,-1.,0.));
#9858=DIRECTION('ref_axis',(1.,0.,0.));
#9859=DIRECTION('center_axis',(0.,1.,0.));
#9860=DIRECTION('ref_axis',(1.,0.,0.));
#9861=DIRECTION('',(0.,-1.,0.));
#9862=DIRECTION('center_axis',(0.,-1.,0.));
#9863=DIRECTION('ref_axis',(1.,0.,0.));
#9864=DIRECTION('center_axis',(0.,1.,0.));
#9865=DIRECTION('ref_axis',(1.,0.,0.));
#9866=DIRECTION('center_axis',(0.,1.,0.));
#9867=DIRECTION('ref_axis',(1.,0.,0.));
#9868=DIRECTION('',(0.,-1.,0.));
#9869=DIRECTION('center_axis',(0.,1.,0.));
#9870=DIRECTION('ref_axis',(1.,0.,0.));
#9871=DIRECTION('center_axis',(0.,1.,0.));
#9872=DIRECTION('ref_axis',(1.,0.,0.));
#9873=DIRECTION('center_axis',(0.,1.,0.));
#9874=DIRECTION('ref_axis',(1.,0.,0.));
#9875=DIRECTION('axis',(0.,0.,1.));
#9876=DIRECTION('refdir',(1.,0.,0.));
#9877=DIRECTION('center_axis',(0.,1.,0.));
#9878=DIRECTION('ref_axis',(1.,0.,0.));
#9879=DIRECTION('center_axis',(0.,1.,0.));
#9880=DIRECTION('ref_axis',(1.,0.,0.));
#9881=DIRECTION('',(0.,1.,0.));
#9882=DIRECTION('center_axis',(0.,-1.,0.));
#9883=DIRECTION('ref_axis',(1.,0.,0.));
#9884=DIRECTION('center_axis',(0.,1.,0.));
#9885=DIRECTION('ref_axis',(1.,0.,0.));
#9886=DIRECTION('center_axis',(0.,1.,0.));
#9887=DIRECTION('ref_axis',(1.,0.,0.));
#9888=DIRECTION('',(0.,1.,0.));
#9889=DIRECTION('center_axis',(0.,-1.,0.));
#9890=DIRECTION('ref_axis',(1.,0.,0.));
#9891=DIRECTION('center_axis',(0.,1.,0.));
#9892=DIRECTION('ref_axis',(1.,0.,0.));
#9893=DIRECTION('center_axis',(0.,1.,0.));
#9894=DIRECTION('ref_axis',(1.,0.,0.));
#9895=DIRECTION('',(0.,1.,0.));
#9896=DIRECTION('center_axis',(0.,-1.,0.));
#9897=DIRECTION('ref_axis',(1.,0.,0.));
#9898=DIRECTION('center_axis',(0.,1.,0.));
#9899=DIRECTION('ref_axis',(1.,0.,0.));
#9900=DIRECTION('center_axis',(0.,1.,0.));
#9901=DIRECTION('ref_axis',(1.,0.,0.));
#9902=DIRECTION('',(0.,1.,0.));
#9903=DIRECTION('center_axis',(0.,-1.,0.));
#9904=DIRECTION('ref_axis',(1.,0.,0.));
#9905=DIRECTION('center_axis',(0.,1.,0.));
#9906=DIRECTION('ref_axis',(1.,0.,0.));
#9907=DIRECTION('center_axis',(0.,1.,0.));
#9908=DIRECTION('ref_axis',(1.,0.,0.));
#9909=DIRECTION('',(0.,-1.,0.));
#9910=DIRECTION('center_axis',(0.,1.,0.));
#9911=DIRECTION('ref_axis',(1.,0.,0.));
#9912=DIRECTION('center_axis',(0.,1.,0.));
#9913=DIRECTION('ref_axis',(1.,0.,0.));
#9914=DIRECTION('center_axis',(0.,-1.,0.));
#9915=DIRECTION('ref_axis',(1.,0.,0.));
#9916=DIRECTION('center_axis',(0.,1.,0.));
#9917=DIRECTION('ref_axis',(1.,0.,0.));
#9918=DIRECTION('center_axis',(0.,-1.,0.));
#9919=DIRECTION('ref_axis',(1.,0.,0.));
#9920=DIRECTION('',(0.,-1.,0.));
#9921=DIRECTION('center_axis',(0.,1.,0.));
#9922=DIRECTION('ref_axis',(1.,0.,0.));
#9923=DIRECTION('center_axis',(0.,1.,0.));
#9924=DIRECTION('ref_axis',(1.,0.,0.));
#9925=DIRECTION('',(0.,-1.,0.));
#9926=DIRECTION('center_axis',(0.,1.,0.));
#9927=DIRECTION('ref_axis',(1.,0.,0.));
#9928=DIRECTION('center_axis',(0.,1.,0.));
#9929=DIRECTION('ref_axis',(1.,0.,0.));
#9930=DIRECTION('center_axis',(0.,1.,0.));
#9931=DIRECTION('ref_axis',(1.,0.,0.));
#9932=DIRECTION('axis',(0.,0.,1.));
#9933=DIRECTION('refdir',(1.,0.,0.));
#9934=DIRECTION('center_axis',(0.,0.,1.));
#9935=DIRECTION('ref_axis',(1.,0.,0.));
#9936=DIRECTION('center_axis',(0.,0.,1.));
#9937=DIRECTION('ref_axis',(1.,0.,0.));
#9938=DIRECTION('',(0.,0.,1.));
#9939=DIRECTION('center_axis',(0.,0.,-1.));
#9940=DIRECTION('ref_axis',(1.,0.,0.));
#9941=DIRECTION('center_axis',(0.,0.,1.));
#9942=DIRECTION('ref_axis',(1.,0.,0.));
#9943=DIRECTION('center_axis',(0.,0.,1.));
#9944=DIRECTION('ref_axis',(1.,0.,0.));
#9945=DIRECTION('center_axis',(0.,0.,1.));
#9946=DIRECTION('ref_axis',(1.,0.,0.));
#9947=DIRECTION('',(0.,0.,1.));
#9948=DIRECTION('center_axis',(0.,0.,-1.));
#9949=DIRECTION('ref_axis',(1.,0.,0.));
#9950=DIRECTION('center_axis',(0.,0.,1.));
#9951=DIRECTION('ref_axis',(1.,0.,0.));
#9952=DIRECTION('center_axis',(0.,0.,1.));
#9953=DIRECTION('ref_axis',(1.,0.,0.));
#9954=DIRECTION('center_axis',(0.,0.,1.));
#9955=DIRECTION('ref_axis',(1.,0.,0.));
#9956=DIRECTION('',(0.,0.,1.));
#9957=DIRECTION('center_axis',(0.,0.,-1.));
#9958=DIRECTION('ref_axis',(1.,0.,0.));
#9959=DIRECTION('center_axis',(0.,0.,1.));
#9960=DIRECTION('ref_axis',(1.,0.,0.));
#9961=DIRECTION('center_axis',(0.,0.,1.));
#9962=DIRECTION('ref_axis',(1.,0.,0.));
#9963=DIRECTION('center_axis',(0.,0.,1.));
#9964=DIRECTION('ref_axis',(1.,0.,0.));
#9965=DIRECTION('center_axis',(0.,0.,1.));
#9966=DIRECTION('ref_axis',(1.,0.,0.));
#9967=DIRECTION('',(0.,0.,1.));
#9968=DIRECTION('center_axis',(0.,0.,-1.));
#9969=DIRECTION('ref_axis',(1.,0.,0.));
#9970=DIRECTION('center_axis',(0.,0.,1.));
#9971=DIRECTION('ref_axis',(1.,0.,0.));
#9972=DIRECTION('center_axis',(0.,0.,1.));
#9973=DIRECTION('ref_axis',(1.,0.,0.));
#9974=DIRECTION('center_axis',(0.,0.,1.));
#9975=DIRECTION('ref_axis',(1.,0.,0.));
#9976=DIRECTION('center_axis',(0.,0.,1.));
#9977=DIRECTION('ref_axis',(1.,0.,0.));
#9978=DIRECTION('',(0.,0.,1.));
#9979=DIRECTION('center_axis',(0.,0.,-1.));
#9980=DIRECTION('ref_axis',(1.,0.,0.));
#9981=DIRECTION('center_axis',(0.,0.,1.));
#9982=DIRECTION('ref_axis',(1.,0.,0.));
#9983=DIRECTION('center_axis',(0.,0.,1.));
#9984=DIRECTION('ref_axis',(1.,0.,0.));
#9985=DIRECTION('center_axis',(0.,0.,1.));
#9986=DIRECTION('ref_axis',(1.,0.,0.));
#9987=DIRECTION('center_axis',(0.,0.,1.));
#9988=DIRECTION('ref_axis',(1.,0.,0.));
#9989=DIRECTION('',(0.,0.,1.));
#9990=DIRECTION('center_axis',(0.,0.,-1.));
#9991=DIRECTION('ref_axis',(1.,0.,0.));
#9992=DIRECTION('center_axis',(0.,0.,1.));
#9993=DIRECTION('ref_axis',(1.,0.,0.));
#9994=DIRECTION('center_axis',(0.,0.,1.));
#9995=DIRECTION('ref_axis',(1.,0.,0.));
#9996=DIRECTION('center_axis',(0.,0.,1.));
#9997=DIRECTION('ref_axis',(1.,0.,0.));
#9998=DIRECTION('center_axis',(0.,0.,1.));
#9999=DIRECTION('ref_axis',(1.,0.,0.));
#10000=DIRECTION('',(0.,0.,1.));
#10001=DIRECTION('center_axis',(0.,0.,1.));
#10002=DIRECTION('ref_axis',(1.,0.,0.));
#10003=DIRECTION('center_axis',(0.,0.,1.));
#10004=DIRECTION('ref_axis',(1.,0.,0.));
#10005=DIRECTION('',(0.,0.,1.));
#10006=DIRECTION('center_axis',(0.,0.,1.));
#10007=DIRECTION('ref_axis',(1.,0.,0.));
#10008=DIRECTION('center_axis',(0.,0.,1.));
#10009=DIRECTION('ref_axis',(1.,0.,0.));
#10010=DIRECTION('',(0.,0.,1.));
#10011=DIRECTION('center_axis',(0.,0.,1.));
#10012=DIRECTION('ref_axis',(1.,0.,0.));
#10013=DIRECTION('center_axis',(0.,0.,1.));
#10014=DIRECTION('ref_axis',(1.,0.,0.));
#10015=DIRECTION('',(0.,0.,1.));
#10016=DIRECTION('center_axis',(0.,1.,0.));
#10017=DIRECTION('ref_axis',(-1.,0.,0.));
#10018=DIRECTION('',(-1.,0.,0.));
#10019=DIRECTION('',(0.,0.,1.));
#10020=DIRECTION('',(-1.,0.,0.));
#10021=DIRECTION('',(0.,0.,1.));
#10022=DIRECTION('center_axis',(1.,0.,0.));
#10023=DIRECTION('ref_axis',(0.,1.,0.));
#10024=DIRECTION('',(0.,1.,0.));
#10025=DIRECTION('',(0.,1.,0.));
#10026=DIRECTION('',(0.,0.,1.));
#10027=DIRECTION('center_axis',(0.,-1.,0.));
#10028=DIRECTION('ref_axis',(1.,0.,0.));
#10029=DIRECTION('',(1.,0.,0.));
#10030=DIRECTION('',(1.,0.,0.));
#10031=DIRECTION('',(0.,0.,1.));
#10032=DIRECTION('center_axis',(-1.,0.,0.));
#10033=DIRECTION('ref_axis',(0.,-1.,0.));
#10034=DIRECTION('',(0.,-1.,0.));
#10035=DIRECTION('',(0.,-1.,0.));
#10036=DIRECTION('center_axis',(0.,0.,1.));
#10037=DIRECTION('ref_axis',(1.,0.,0.));
#10038=DIRECTION('center_axis',(0.,0.,1.));
#10039=DIRECTION('ref_axis',(1.,0.,0.));
#10040=DIRECTION('axis',(0.,0.,1.));
#10041=DIRECTION('refdir',(1.,0.,0.));
#10042=DIRECTION('center_axis',(0.,0.,1.));
#10043=DIRECTION('ref_axis',(1.,0.,0.));
#10044=DIRECTION('center_axis',(0.,0.,1.));
#10045=DIRECTION('ref_axis',(1.,0.,0.));
#10046=DIRECTION('',(0.,0.,1.));
#10047=DIRECTION('center_axis',(0.,0.,-1.));
#10048=DIRECTION('ref_axis',(1.,0.,0.));
#10049=DIRECTION('center_axis',(0.,0.,1.));
#10050=DIRECTION('ref_axis',(1.,0.,0.));
#10051=DIRECTION('center_axis',(0.,0.,1.));
#10052=DIRECTION('ref_axis',(1.,0.,0.));
#10053=DIRECTION('',(0.,0.,1.));
#10054=DIRECTION('center_axis',(0.,0.,-1.));
#10055=DIRECTION('ref_axis',(1.,0.,0.));
#10056=DIRECTION('center_axis',(0.,0.,1.));
#10057=DIRECTION('ref_axis',(1.,0.,0.));
#10058=DIRECTION('',(-1.,0.,0.));
#10059=DIRECTION('',(0.,1.,0.));
#10060=DIRECTION('',(1.,0.,0.));
#10061=DIRECTION('',(0.,1.,0.));
#10062=DIRECTION('center_axis',(0.,1.,0.));
#10063=DIRECTION('ref_axis',(0.,0.,1.));
#10064=DIRECTION('',(0.,0.,-1.));
#10065=DIRECTION('',(-1.,0.,0.));
#10066=DIRECTION('',(0.,0.,1.));
#10067=DIRECTION('center_axis',(0.,1.,0.));
#10068=DIRECTION('ref_axis',(-1.,0.,0.));
#10069=DIRECTION('',(0.,0.,1.));
#10070=DIRECTION('',(-1.,0.,0.));
#10071=DIRECTION('',(0.,0.,1.));
#10072=DIRECTION('center_axis',(0.,0.,1.));
#10073=DIRECTION('ref_axis',(1.,0.,0.));
#10074=DIRECTION('',(-1.,0.,0.));
#10075=DIRECTION('',(0.,1.,0.));
#10076=DIRECTION('',(1.,0.,0.));
#10077=DIRECTION('',(0.,1.,0.));
#10078=DIRECTION('center_axis',(0.,1.,0.));
#10079=DIRECTION('ref_axis',(1.,0.,0.));
#10080=DIRECTION('',(0.,0.,-1.));
#10081=DIRECTION('',(1.,0.,0.));
#10082=DIRECTION('',(0.,0.,1.));
#10083=DIRECTION('center_axis',(1.,0.,0.));
#10084=DIRECTION('ref_axis',(0.,1.,0.));
#10085=DIRECTION('',(0.,1.,0.));
#10086=DIRECTION('',(0.,1.,0.));
#10087=DIRECTION('',(0.,0.,1.));
#10088=DIRECTION('center_axis',(0.,-1.,0.));
#10089=DIRECTION('ref_axis',(1.,0.,0.));
#10090=DIRECTION('',(1.,0.,0.));
#10091=DIRECTION('',(0.,0.,1.));
#10092=DIRECTION('center_axis',(-1.,0.,0.));
#10093=DIRECTION('ref_axis',(0.,-1.,0.));
#10094=DIRECTION('',(0.,-1.,0.));
#10095=DIRECTION('',(0.,-1.,0.));
#10096=DIRECTION('center_axis',(0.,0.,1.));
#10097=DIRECTION('ref_axis',(1.,0.,0.));
#10098=DIRECTION('center_axis',(0.,0.,1.));
#10099=DIRECTION('ref_axis',(1.,0.,0.));
#10100=DIRECTION('axis',(0.,0.,1.));
#10101=DIRECTION('refdir',(1.,0.,0.));
#10102=DIRECTION('center_axis',(0.,0.,1.));
#10103=DIRECTION('ref_axis',(1.,0.,0.));
#10104=DIRECTION('center_axis',(0.,0.,1.));
#10105=DIRECTION('ref_axis',(1.,0.,0.));
#10106=DIRECTION('',(0.,0.,1.));
#10107=DIRECTION('center_axis',(0.,0.,-1.));
#10108=DIRECTION('ref_axis',(1.,0.,0.));
#10109=DIRECTION('center_axis',(0.,0.,1.));
#10110=DIRECTION('ref_axis',(1.,0.,0.));
#10111=DIRECTION('center_axis',(0.,0.,1.));
#10112=DIRECTION('ref_axis',(1.,0.,0.));
#10113=DIRECTION('center_axis',(0.,0.,1.));
#10114=DIRECTION('ref_axis',(1.,0.,0.));
#10115=DIRECTION('center_axis',(0.,0.,1.));
#10116=DIRECTION('ref_axis',(1.,0.,0.));
#10117=DIRECTION('',(0.,0.,1.));
#10118=DIRECTION('center_axis',(0.,0.,1.));
#10119=DIRECTION('ref_axis',(1.,0.,0.));
#10120=DIRECTION('center_axis',(0.,0.,1.));
#10121=DIRECTION('ref_axis',(1.,0.,0.));
#10122=DIRECTION('',(0.,-1.,0.));
#10123=DIRECTION('',(-1.,0.,0.));
#10124=DIRECTION('',(0.,1.,0.));
#10125=DIRECTION('',(1.,0.,0.));
#10126=DIRECTION('center_axis',(0.,0.,1.));
#10127=DIRECTION('ref_axis',(1.,0.,0.));
#10128=DIRECTION('',(0.,0.,-1.));
#10129=DIRECTION('center_axis',(0.,0.,1.));
#10130=DIRECTION('ref_axis',(1.,0.,0.));
#10131=DIRECTION('center_axis',(1.,0.,0.));
#10132=DIRECTION('ref_axis',(0.,1.,0.));
#10133=DIRECTION('',(0.,0.,1.));
#10134=DIRECTION('',(0.,1.,0.));
#10135=DIRECTION('',(0.,0.,1.));
#10136=DIRECTION('',(0.,1.,0.));
#10137=DIRECTION('',(0.,0.,-1.));
#10138=DIRECTION('',(0.,1.,0.));
#10139=DIRECTION('',(0.,0.,1.));
#10140=DIRECTION('center_axis',(0.,1.,0.));
#10141=DIRECTION('ref_axis',(-1.,0.,0.));
#10142=DIRECTION('',(0.,0.,1.));
#10143=DIRECTION('',(-1.,0.,0.));
#10144=DIRECTION('',(0.,0.,-1.));
#10145=DIRECTION('',(-1.,0.,0.));
#10146=DIRECTION('',(0.,0.,1.));
#10147=DIRECTION('',(-1.,0.,0.));
#10148=DIRECTION('center_axis',(0.,0.,1.));
#10149=DIRECTION('ref_axis',(1.,0.,0.));
#10150=DIRECTION('center_axis',(0.,0.,1.));
#10151=DIRECTION('ref_axis',(1.,0.,0.));
#10152=DIRECTION('',(0.,0.,1.));
#10153=DIRECTION('center_axis',(0.,0.,-1.));
#10154=DIRECTION('ref_axis',(1.,0.,0.));
#10155=DIRECTION('center_axis',(0.,0.,1.));
#10156=DIRECTION('ref_axis',(1.,0.,0.));
#10157=DIRECTION('center_axis',(0.,0.,1.));
#10158=DIRECTION('ref_axis',(1.,0.,0.));
#10159=DIRECTION('center_axis',(0.,0.,1.));
#10160=DIRECTION('ref_axis',(1.,0.,0.));
#10161=DIRECTION('center_axis',(0.,0.,1.));
#10162=DIRECTION('ref_axis',(1.,0.,0.));
#10163=DIRECTION('',(0.,0.,1.));
#10164=DIRECTION('center_axis',(0.,0.,1.));
#10165=DIRECTION('ref_axis',(1.,0.,0.));
#10166=DIRECTION('center_axis',(0.,0.,1.));
#10167=DIRECTION('ref_axis',(1.,0.,0.));
#10168=DIRECTION('',(1.,0.,0.));
#10169=DIRECTION('',(0.,-1.,0.));
#10170=DIRECTION('',(-1.,0.,0.));
#10171=DIRECTION('center_axis',(0.,0.,1.));
#10172=DIRECTION('ref_axis',(1.,0.,0.));
#10173=DIRECTION('',(0.,0.,-1.));
#10174=DIRECTION('center_axis',(0.,0.,1.));
#10175=DIRECTION('ref_axis',(1.,0.,0.));
#10176=DIRECTION('center_axis',(0.,1.,0.));
#10177=DIRECTION('ref_axis',(0.,0.,1.));
#10178=DIRECTION('',(0.,0.,1.));
#10179=DIRECTION('',(-1.,0.,0.));
#10180=DIRECTION('center_axis',(-1.,0.,0.));
#10181=DIRECTION('ref_axis',(0.,0.,1.));
#10182=DIRECTION('',(0.,0.,-1.));
#10183=DIRECTION('',(0.,-1.,0.));
#10184=DIRECTION('center_axis',(0.,0.,1.));
#10185=DIRECTION('ref_axis',(1.,0.,0.));
#10186=DIRECTION('center_axis',(0.,0.,1.));
#10187=DIRECTION('ref_axis',(1.,0.,0.));
#10188=DIRECTION('',(0.,0.,1.));
#10189=DIRECTION('center_axis',(0.,0.,-1.));
#10190=DIRECTION('ref_axis',(1.,0.,0.));
#10191=DIRECTION('center_axis',(0.,0.,1.));
#10192=DIRECTION('ref_axis',(1.,0.,0.));
#10193=DIRECTION('center_axis',(0.,0.,1.));
#10194=DIRECTION('ref_axis',(1.,0.,0.));
#10195=DIRECTION('center_axis',(0.,0.,1.));
#10196=DIRECTION('ref_axis',(1.,0.,0.));
#10197=DIRECTION('center_axis',(0.,0.,1.));
#10198=DIRECTION('ref_axis',(1.,0.,0.));
#10199=DIRECTION('',(0.,0.,1.));
#10200=DIRECTION('center_axis',(0.,0.,1.));
#10201=DIRECTION('ref_axis',(1.,0.,0.));
#10202=DIRECTION('center_axis',(0.,0.,1.));
#10203=DIRECTION('ref_axis',(1.,0.,0.));
#10204=DIRECTION('',(0.,1.,0.));
#10205=DIRECTION('',(1.,0.,0.));
#10206=DIRECTION('',(0.,-1.,0.));
#10207=DIRECTION('center_axis',(0.,0.,1.));
#10208=DIRECTION('ref_axis',(1.,0.,0.));
#10209=DIRECTION('',(0.,0.,-1.));
#10210=DIRECTION('center_axis',(0.,0.,1.));
#10211=DIRECTION('ref_axis',(1.,0.,0.));
#10212=DIRECTION('center_axis',(0.,1.,0.));
#10213=DIRECTION('ref_axis',(1.,0.,0.));
#10214=DIRECTION('',(0.,0.,1.));
#10215=DIRECTION('',(1.,0.,0.));
#10216=DIRECTION('',(0.,0.,-1.));
#10217=DIRECTION('center_axis',(1.,0.,0.));
#10218=DIRECTION('ref_axis',(0.,0.,-1.));
#10219=DIRECTION('',(0.,1.,0.));
#10220=DIRECTION('center_axis',(0.,0.,1.));
#10221=DIRECTION('ref_axis',(1.,0.,0.));
#10222=DIRECTION('center_axis',(0.,0.,1.));
#10223=DIRECTION('ref_axis',(1.,0.,0.));
#10224=DIRECTION('',(0.,0.,1.));
#10225=DIRECTION('center_axis',(0.,0.,-1.));
#10226=DIRECTION('ref_axis',(1.,0.,0.));
#10227=DIRECTION('center_axis',(0.,0.,1.));
#10228=DIRECTION('ref_axis',(1.,0.,0.));
#10229=DIRECTION('center_axis',(0.,0.,1.));
#10230=DIRECTION('ref_axis',(1.,0.,0.));
#10231=DIRECTION('center_axis',(0.,0.,1.));
#10232=DIRECTION('ref_axis',(1.,0.,0.));
#10233=DIRECTION('center_axis',(0.,0.,1.));
#10234=DIRECTION('ref_axis',(1.,0.,0.));
#10235=DIRECTION('',(0.,0.,1.));
#10236=DIRECTION('center_axis',(0.,0.,1.));
#10237=DIRECTION('ref_axis',(1.,0.,0.));
#10238=DIRECTION('center_axis',(0.,0.,1.));
#10239=DIRECTION('ref_axis',(1.,0.,0.));
#10240=DIRECTION('',(-1.,0.,0.));
#10241=DIRECTION('',(0.,1.,0.));
#10242=DIRECTION('',(1.,0.,0.));
#10243=DIRECTION('',(0.,-1.,0.));
#10244=DIRECTION('center_axis',(0.,0.,1.));
#10245=DIRECTION('ref_axis',(1.,0.,0.));
#10246=DIRECTION('',(0.,0.,-1.));
#10247=DIRECTION('center_axis',(0.,0.,1.));
#10248=DIRECTION('ref_axis',(1.,0.,0.));
#10249=DIRECTION('center_axis',(0.,-1.,0.));
#10250=DIRECTION('ref_axis',(1.,0.,0.));
#10251=DIRECTION('',(1.,0.,0.));
#10252=DIRECTION('',(0.,0.,1.));
#10253=DIRECTION('',(0.,0.,1.));
#10254=DIRECTION('',(1.,0.,0.));
#10255=DIRECTION('center_axis',(1.,0.,0.));
#10256=DIRECTION('ref_axis',(0.,0.,-1.));
#10257=DIRECTION('',(0.,0.,-1.));
#10258=DIRECTION('',(0.,1.,0.));
#10259=DIRECTION('center_axis',(0.,-1.,0.));
#10260=DIRECTION('ref_axis',(1.,0.,0.));
#10261=DIRECTION('',(1.,0.,0.));
#10262=DIRECTION('',(0.,0.,1.));
#10263=DIRECTION('',(-1.,0.,0.));
#10264=DIRECTION('',(0.,0.,1.));
#10265=DIRECTION('center_axis',(1.,0.,0.));
#10266=DIRECTION('ref_axis',(0.,1.,0.));
#10267=DIRECTION('',(0.,1.,0.));
#10268=DIRECTION('',(0.,-1.,0.));
#10269=DIRECTION('',(0.,0.,1.));
#10270=DIRECTION('center_axis',(0.,1.,0.));
#10271=DIRECTION('ref_axis',(-1.,0.,0.));
#10272=DIRECTION('',(-1.,0.,0.));
#10273=DIRECTION('',(1.,0.,0.));
#10274=DIRECTION('',(0.,0.,1.));
#10275=DIRECTION('center_axis',(-1.,0.,0.));
#10276=DIRECTION('ref_axis',(0.,-1.,0.));
#10277=DIRECTION('',(0.,-1.,0.));
#10278=DIRECTION('',(0.,1.,0.));
#10279=DIRECTION('center_axis',(-1.,0.,0.));
#10280=DIRECTION('ref_axis',(0.,0.,1.));
#10281=DIRECTION('',(0.,0.,-1.));
#10282=DIRECTION('',(0.,-1.,0.));
#10283=DIRECTION('center_axis',(0.,0.,-1.));
#10284=DIRECTION('ref_axis',(-1.,0.,0.));
#10285=DIRECTION('center_axis',(0.,1.,0.));
#10286=DIRECTION('ref_axis',(1.,0.,0.));
#10287=DIRECTION('',(1.,0.,0.));
#10288=DIRECTION('center_axis',(0.,0.,1.));
#10289=DIRECTION('ref_axis',(1.,0.,0.));
#10290=DIRECTION('',(-1.,0.,0.));
#10291=DIRECTION('',(0.,-1.,0.));
#10292=DIRECTION('center_axis',(0.,0.,-1.));
#10293=DIRECTION('ref_axis',(-1.,0.,0.));
#10294=DIRECTION('center_axis',(0.,0.,-1.));
#10295=DIRECTION('ref_axis',(-1.,0.,0.));
#10296=DIRECTION('center_axis',(0.,1.,0.));
#10297=DIRECTION('ref_axis',(0.,0.,1.));
#10298=DIRECTION('',(0.,0.,1.));
#10299=DIRECTION('center_axis',(0.,0.,-1.));
#10300=DIRECTION('ref_axis',(-1.,0.,0.));
#10301=DIRECTION('center_axis',(-1.,0.,0.));
#10302=DIRECTION('ref_axis',(0.,-1.,0.));
#10303=DIRECTION('',(0.,-1.,0.));
#10304=DIRECTION('center_axis',(0.,0.,1.));
#10305=DIRECTION('ref_axis',(1.,0.,0.));
#10306=DIRECTION('axis',(0.,0.,1.));
#10307=DIRECTION('refdir',(1.,0.,0.));
#10308=DIRECTION('center_axis',(0.,1.,0.));
#10309=DIRECTION('ref_axis',(-1.,0.,0.));
#10310=DIRECTION('',(-1.,0.,0.));
#10311=DIRECTION('',(0.,0.,1.));
#10312=DIRECTION('',(-1.,0.,0.));
#10313=DIRECTION('',(0.,0.,1.));
#10314=DIRECTION('center_axis',(1.,0.,0.));
#10315=DIRECTION('ref_axis',(0.,1.,0.));
#10316=DIRECTION('',(0.,1.,0.));
#10317=DIRECTION('',(0.,1.,0.));
#10318=DIRECTION('',(0.,0.,1.));
#10319=DIRECTION('center_axis',(0.,-1.,0.));
#10320=DIRECTION('ref_axis',(1.,0.,0.));
#10321=DIRECTION('',(1.,0.,0.));
#10322=DIRECTION('',(1.,0.,0.));
#10323=DIRECTION('',(0.,0.,1.));
#10324=DIRECTION('center_axis',(-1.,0.,0.));
#10325=DIRECTION('ref_axis',(0.,-1.,0.));
#10326=DIRECTION('',(0.,-1.,0.));
#10327=DIRECTION('',(0.,-1.,0.));
#10328=DIRECTION('center_axis',(0.,0.,1.));
#10329=DIRECTION('ref_axis',(1.,0.,0.));
#10330=DIRECTION('center_axis',(0.,0.,1.));
#10331=DIRECTION('ref_axis',(1.,0.,0.));
#10332=DIRECTION('axis',(0.,0.,1.));
#10333=DIRECTION('refdir',(1.,0.,0.));
#10334=DIRECTION('center_axis',(0.,1.,0.));
#10335=DIRECTION('ref_axis',(-1.,0.,0.));
#10336=DIRECTION('',(-1.,0.,0.));
#10337=DIRECTION('',(0.,0.,1.));
#10338=DIRECTION('',(-1.,0.,0.));
#10339=DIRECTION('',(0.,0.,1.));
#10340=DIRECTION('center_axis',(1.,0.,0.));
#10341=DIRECTION('ref_axis',(0.,1.,0.));
#10342=DIRECTION('',(0.,1.,0.));
#10343=DIRECTION('',(0.,1.,0.));
#10344=DIRECTION('',(0.,0.,1.));
#10345=DIRECTION('center_axis',(0.,-1.,0.));
#10346=DIRECTION('ref_axis',(1.,0.,0.));
#10347=DIRECTION('',(1.,0.,0.));
#10348=DIRECTION('',(1.,0.,0.));
#10349=DIRECTION('',(0.,0.,1.));
#10350=DIRECTION('center_axis',(-1.,0.,0.));
#10351=DIRECTION('ref_axis',(0.,-1.,0.));
#10352=DIRECTION('',(0.,-1.,0.));
#10353=DIRECTION('',(0.,-1.,0.));
#10354=DIRECTION('center_axis',(0.,0.,1.));
#10355=DIRECTION('ref_axis',(1.,0.,0.));
#10356=DIRECTION('center_axis',(0.,0.,1.));
#10357=DIRECTION('ref_axis',(1.,0.,0.));
#10358=DIRECTION('axis',(0.,0.,1.));
#10359=DIRECTION('refdir',(1.,0.,0.));
#10360=DIRECTION('center_axis',(0.866025403784439,0.,-0.5));
#10361=DIRECTION('ref_axis',(0.5,0.,0.866025403784439));
#10362=DIRECTION('',(-0.5,0.,-0.866025403784439));
#10363=DIRECTION('',(0.,-1.,0.));
#10364=DIRECTION('',(0.5,0.,0.866025403784439));
#10365=DIRECTION('',(0.,-1.,0.));
#10366=DIRECTION('center_axis',(1.92296268638356E-16,0.,-1.));
#10367=DIRECTION('ref_axis',(1.,0.,1.92296268638356E-16));
#10368=DIRECTION('',(-1.,0.,-1.92296268638356E-16));
#10369=DIRECTION('',(0.,-1.,0.));
#10370=DIRECTION('',(1.,0.,1.92296268638356E-16));
#10371=DIRECTION('center_axis',(-0.866025403784439,0.,-0.5));
#10372=DIRECTION('ref_axis',(0.5,0.,-0.866025403784439));
#10373=DIRECTION('',(-0.5,0.,0.866025403784438));
#10374=DIRECTION('',(0.,-1.,0.));
#10375=DIRECTION('',(0.5,0.,-0.866025403784438));
#10376=DIRECTION('center_axis',(-0.866025403784439,0.,0.5));
#10377=DIRECTION('ref_axis',(-0.5,0.,-0.866025403784439));
#10378=DIRECTION('',(0.5,0.,0.866025403784439));
#10379=DIRECTION('',(0.,-1.,0.));
#10380=DIRECTION('',(-0.5,0.,-0.866025403784439));
#10381=DIRECTION('center_axis',(-1.92296268638356E-16,0.,1.));
#10382=DIRECTION('ref_axis',(-1.,0.,-1.92296268638356E-16));
#10383=DIRECTION('',(1.,0.,1.92296268638356E-16));
#10384=DIRECTION('',(0.,-1.,0.));
#10385=DIRECTION('',(-1.,0.,-1.92296268638356E-16));
#10386=DIRECTION('center_axis',(0.866025403784439,0.,0.5));
#10387=DIRECTION('ref_axis',(-0.5,0.,0.866025403784439));
#10388=DIRECTION('',(0.5,0.,-0.866025403784439));
#10389=DIRECTION('',(-0.5,0.,0.866025403784439));
#10390=DIRECTION('center_axis',(0.,1.,0.));
#10391=DIRECTION('ref_axis',(1.,0.,0.));
#10392=DIRECTION('center_axis',(0.,-1.,0.));
#10393=DIRECTION('ref_axis',(0.,0.,-1.));
#10394=DIRECTION('center_axis',(0.,1.,0.));
#10395=DIRECTION('ref_axis',(1.,0.,0.));
#10396=DIRECTION('center_axis',(0.,1.,0.));
#10397=DIRECTION('ref_axis',(1.,0.,0.));
#10398=DIRECTION('center_axis',(0.,1.,0.));
#10399=DIRECTION('ref_axis',(0.,0.,1.));
#10400=DIRECTION('center_axis',(0.,-1.,0.));
#10401=DIRECTION('ref_axis',(1.,0.,0.));
#10402=DIRECTION('center_axis',(0.,-1.,0.));
#10403=DIRECTION('ref_axis',(1.,0.,0.));
#10404=DIRECTION('center_axis',(0.,-1.,0.));
#10405=DIRECTION('ref_axis',(1.,0.,0.));
#10406=DIRECTION('',(0.707106781186548,0.707106781186547,8.65956056235494E-17));
#10407=DIRECTION('center_axis',(0.,-1.,0.));
#10408=DIRECTION('ref_axis',(1.,0.,0.));
#10409=DIRECTION('center_axis',(0.,-1.,0.));
#10410=DIRECTION('ref_axis',(1.,0.,0.));
#10411=DIRECTION('',(0.,1.,0.));
#10412=DIRECTION('center_axis',(0.,1.,0.));
#10413=DIRECTION('ref_axis',(1.,0.,0.));
#10414=DIRECTION('center_axis',(0.,-1.,0.));
#10415=DIRECTION('ref_axis',(1.,0.,0.));
#10416=DIRECTION('',(-0.707106781186547,0.707106781186548,-8.65956056235493E-17));
#10417=DIRECTION('center_axis',(0.,-1.,0.));
#10418=DIRECTION('ref_axis',(0.,0.,-1.));
#10419=DIRECTION('center_axis',(0.,-1.,0.));
#10420=DIRECTION('ref_axis',(1.,0.,0.));
#10421=DIRECTION('center_axis',(0.,1.,0.));
#10422=DIRECTION('ref_axis',(1.,0.,0.));
#10423=DIRECTION('center_axis',(0.,1.,0.));
#10424=DIRECTION('ref_axis',(1.,0.,0.));
#10425=DIRECTION('',(-0.447213595499958,0.894427190999916,-5.47678698264203E-17));
#10426=DIRECTION('center_axis',(0.,-1.,0.));
#10427=DIRECTION('ref_axis',(1.,0.,0.));
#10428=DIRECTION('',(0.,1.,0.));
#10429=DIRECTION('axis',(0.,0.,1.));
#10430=DIRECTION('refdir',(1.,0.,0.));
#10431=DIRECTION('axis',(0.,0.,1.));
#10432=DIRECTION('refdir',(1.,0.,0.));
#10433=DIRECTION('center_axis',(0.,-1.,0.));
#10434=DIRECTION('ref_axis',(0.,0.,-1.));
#10435=DIRECTION('center_axis',(0.,-1.,0.));
#10436=DIRECTION('ref_axis',(1.,0.,0.));
#10437=DIRECTION('center_axis',(0.,-1.,0.));
#10438=DIRECTION('ref_axis',(1.,0.,0.));
#10439=DIRECTION('center_axis',(1.,0.,1.22464679914735E-16));
#10440=DIRECTION('ref_axis',(-1.22464679914735E-16,0.,1.));
#10441=DIRECTION('center_axis',(0.,1.,0.));
#10442=DIRECTION('ref_axis',(1.,0.,0.));
#10443=DIRECTION('center_axis',(0.,1.,0.));
#10444=DIRECTION('ref_axis',(1.,0.,0.));
#10445=DIRECTION('center_axis',(0.,-1.,0.));
#10446=DIRECTION('ref_axis',(1.,0.,0.));
#10447=DIRECTION('',(0.,1.,0.));
#10448=DIRECTION('center_axis',(0.,-1.,0.));
#10449=DIRECTION('ref_axis',(1.,0.,0.));
#10450=DIRECTION('center_axis',(0.,-1.,0.));
#10451=DIRECTION('ref_axis',(1.,0.,0.));
#10452=DIRECTION('center_axis',(0.,-1.,0.));
#10453=DIRECTION('ref_axis',(1.,0.,0.));
#10454=DIRECTION('',(0.,1.,0.));
#10455=DIRECTION('center_axis',(0.,-1.,0.));
#10456=DIRECTION('ref_axis',(1.,0.,0.));
#10457=DIRECTION('center_axis',(0.,1.,0.));
#10458=DIRECTION('ref_axis',(1.,0.,0.));
#10459=DIRECTION('',(-0.707106781186548,0.707106781186547,-8.65956056235493E-17));
#10460=DIRECTION('center_axis',(0.,-1.,0.));
#10461=DIRECTION('ref_axis',(1.,0.,0.));
#10462=DIRECTION('center_axis',(0.,1.,0.));
#10463=DIRECTION('ref_axis',(0.,0.,1.));
#10464=DIRECTION('center_axis',(0.,-1.,0.));
#10465=DIRECTION('ref_axis',(1.,0.,0.));
#10466=DIRECTION('center_axis',(0.,-1.,0.));
#10467=DIRECTION('ref_axis',(1.,0.,0.));
#10468=DIRECTION('',(0.,1.,0.));
#10469=DIRECTION('center_axis',(0.,-1.,0.));
#10470=DIRECTION('ref_axis',(0.,0.,-1.));
#10471=DIRECTION('center_axis',(0.,-1.,0.));
#10472=DIRECTION('ref_axis',(1.,0.,0.));
#10473=DIRECTION('center_axis',(0.,-1.,0.));
#10474=DIRECTION('ref_axis',(1.,0.,0.));
#10475=DIRECTION('',(0.707106781186548,0.707106781186547,8.65956056235493E-17));
#10476=DIRECTION('axis',(0.,0.,1.));
#10477=DIRECTION('refdir',(1.,0.,0.));
#10478=DIRECTION('center_axis',(0.,-1.,0.));
#10479=DIRECTION('ref_axis',(0.,0.,-1.));
#10480=DIRECTION('center_axis',(0.,-1.,0.));
#10481=DIRECTION('ref_axis',(1.,0.,0.));
#10482=DIRECTION('center_axis',(0.,-1.,0.));
#10483=DIRECTION('ref_axis',(1.,0.,0.));
#10484=DIRECTION('center_axis',(1.,0.,1.22464679914735E-16));
#10485=DIRECTION('ref_axis',(-1.22464679914735E-16,0.,1.));
#10486=DIRECTION('center_axis',(0.,1.,0.));
#10487=DIRECTION('ref_axis',(1.,0.,0.));
#10488=DIRECTION('center_axis',(0.,1.,0.));
#10489=DIRECTION('ref_axis',(1.,0.,0.));
#10490=DIRECTION('center_axis',(0.,-1.,0.));
#10491=DIRECTION('ref_axis',(1.,0.,0.));
#10492=DIRECTION('center_axis',(0.,-1.,0.));
#10493=DIRECTION('ref_axis',(1.,0.,0.));
#10494=DIRECTION('',(0.,1.,0.));
#10495=DIRECTION('center_axis',(0.,1.,0.));
#10496=DIRECTION('ref_axis',(0.,0.,1.));
#10497=DIRECTION('center_axis',(0.,-1.,0.));
#10498=DIRECTION('ref_axis',(1.,0.,0.));
#10499=DIRECTION('center_axis',(0.,-1.,0.));
#10500=DIRECTION('ref_axis',(1.,0.,0.));
#10501=DIRECTION('center_axis',(0.,-1.,0.));
#10502=DIRECTION('ref_axis',(1.,0.,0.));
#10503=DIRECTION('center_axis',(0.,-1.,0.));
#10504=DIRECTION('ref_axis',(1.,0.,0.));
#10505=DIRECTION('',(0.707106781186548,0.707106781186547,8.65956056235494E-17));
#10506=DIRECTION('center_axis',(0.,-1.,0.));
#10507=DIRECTION('ref_axis',(1.,0.,0.));
#10508=DIRECTION('center_axis',(0.,-1.,0.));
#10509=DIRECTION('ref_axis',(1.,0.,0.));
#10510=DIRECTION('',(0.,1.,0.));
#10511=DIRECTION('center_axis',(0.,1.,0.));
#10512=DIRECTION('ref_axis',(1.,0.,0.));
#10513=DIRECTION('center_axis',(0.,-1.,0.));
#10514=DIRECTION('ref_axis',(1.,0.,0.));
#10515=DIRECTION('',(-0.707106781186548,0.707106781186547,-8.65956056235494E-17));
#10516=DIRECTION('center_axis',(0.,-1.,0.));
#10517=DIRECTION('ref_axis',(0.,0.,-1.));
#10518=DIRECTION('center_axis',(0.,-1.,0.));
#10519=DIRECTION('ref_axis',(1.,0.,0.));
#10520=DIRECTION('',(0.,1.,0.));
#10521=DIRECTION('axis',(0.,0.,1.));
#10522=DIRECTION('refdir',(1.,0.,0.));
#10523=DIRECTION('center_axis',(0.,0.,1.));
#10524=DIRECTION('ref_axis',(1.,0.,0.));
#10525=DIRECTION('center_axis',(1.22464679914735E-16,-1.,0.));
#10526=DIRECTION('ref_axis',(-1.,-1.22464679914735E-16,0.));
#10527=DIRECTION('center_axis',(0.78183148246803,0.,0.623489801858733));
#10528=DIRECTION('ref_axis',(0.623489801858734,0.,-0.78183148246803));
#10529=DIRECTION('center_axis',(7.63554790147315E-17,-1.,-9.57467422477103E-17));
#10530=DIRECTION('ref_axis',(-0.623489801858734,-1.22464679914735E-16,0.78183148246803));
#10531=DIRECTION('center_axis',(0.974927912181824,0.,-0.222520933956314));
#10532=DIRECTION('ref_axis',(-0.222520933956314,0.,-0.974927912181824));
#10533=DIRECTION('center_axis',(-2.7250954951288E-17,-1.,-1.19394234705288E-16));
#10534=DIRECTION('ref_axis',(0.222520933956314,-1.22464679914735E-16,0.974927912181824));
#10535=DIRECTION('center_axis',(0.433883739117558,0.,-0.900968867902419));
#10536=DIRECTION('ref_axis',(-0.900968867902419,0.,-0.433883739117558));
#10537=DIRECTION('center_axis',(-1.10336864020811E-16,-1.,-5.31354332312403E-17));
#10538=DIRECTION('ref_axis',(0.900968867902419,-1.22464679914735E-16,0.433883739117558));
#10539=DIRECTION('center_axis',(-0.433883739117558,0.,-0.900968867902419));
#10540=DIRECTION('ref_axis',(-0.900968867902419,0.,0.433883739117558));
#10541=DIRECTION('center_axis',(-1.10336864020811E-16,-1.,5.31354332312403E-17));
#10542=DIRECTION('ref_axis',(0.900968867902419,-1.22464679914735E-16,-0.433883739117558));
#10543=DIRECTION('center_axis',(-0.974927912181824,0.,-0.222520933956314));
#10544=DIRECTION('ref_axis',(-0.222520933956315,0.,0.974927912181824));
#10545=DIRECTION('center_axis',(-2.7250954951288E-17,-1.,1.19394234705288E-16));
#10546=DIRECTION('ref_axis',(0.222520933956315,-1.22464679914735E-16,-0.974927912181824));
#10547=DIRECTION('center_axis',(-0.78183148246803,0.,0.623489801858734));
#10548=DIRECTION('ref_axis',(0.623489801858733,0.,0.78183148246803));
#10549=DIRECTION('center_axis',(7.63554790147315E-17,-1.,9.57467422477103E-17));
#10550=DIRECTION('ref_axis',(-0.623489801858733,-1.22464679914735E-16,-0.78183148246803));
#10551=DIRECTION('axis',(0.,0.,1.));
#10552=DIRECTION('refdir',(1.,0.,0.));
#10553=DIRECTION('center_axis',(0.,0.,1.));
#10554=DIRECTION('ref_axis',(1.,0.,0.));
#10555=DIRECTION('center_axis',(0.,-1.,0.));
#10556=DIRECTION('ref_axis',(0.,0.,-1.));
#10557=DIRECTION('center_axis',(0.,-1.,0.));
#10558=DIRECTION('ref_axis',(0.,0.,-1.));
#10559=DIRECTION('center_axis',(0.,1.,0.));
#10560=DIRECTION('ref_axis',(1.,0.,0.));
#10561=DIRECTION('center_axis',(0.,1.,0.));
#10562=DIRECTION('ref_axis',(1.,0.,0.));
#10563=DIRECTION('center_axis',(0.,1.,0.));
#10564=DIRECTION('ref_axis',(1.,0.,0.));
#10565=DIRECTION('center_axis',(0.,1.,0.));
#10566=DIRECTION('ref_axis',(1.,0.,0.));
#10567=DIRECTION('',(0.,-1.,0.));
#10568=DIRECTION('center_axis',(0.,-1.,0.));
#10569=DIRECTION('ref_axis',(1.,0.,0.));
#10570=DIRECTION('center_axis',(0.,1.,0.));
#10571=DIRECTION('ref_axis',(1.,0.,0.));
#10572=DIRECTION('center_axis',(0.,1.,0.));
#10573=DIRECTION('ref_axis',(1.,0.,0.));
#10574=DIRECTION('center_axis',(0.,1.,0.));
#10575=DIRECTION('ref_axis',(1.,0.,0.));
#10576=DIRECTION('center_axis',(0.,1.,0.));
#10577=DIRECTION('ref_axis',(1.,0.,0.));
#10578=DIRECTION('center_axis',(0.,1.,0.));
#10579=DIRECTION('ref_axis',(1.,0.,0.));
#10580=DIRECTION('center_axis',(0.,1.,0.));
#10581=DIRECTION('ref_axis',(1.,0.,0.));
#10582=DIRECTION('center_axis',(0.,-1.,0.));
#10583=DIRECTION('ref_axis',(1.,0.,0.));
#10584=DIRECTION('center_axis',(0.,-1.,0.));
#10585=DIRECTION('ref_axis',(0.,0.,-1.));
#10586=DIRECTION('center_axis',(8.96625347776458E-17,0.,1.));
#10587=DIRECTION('ref_axis',(1.,0.,0.));
#10588=DIRECTION('center_axis',(0.,-1.,0.));
#10589=DIRECTION('ref_axis',(0.,0.,-1.));
#10590=DIRECTION('center_axis',(0.,1.,0.));
#10591=DIRECTION('ref_axis',(1.,0.,0.));
#10592=DIRECTION('center_axis',(0.,-1.,0.));
#10593=DIRECTION('ref_axis',(1.,0.,0.));
#10594=DIRECTION('center_axis',(0.,-1.,0.));
#10595=DIRECTION('ref_axis',(0.,0.,-1.));
#10596=DIRECTION('center_axis',(0.,0.,1.));
#10597=DIRECTION('ref_axis',(1.,0.,0.));
#10598=DIRECTION('center_axis',(0.,-1.,0.));
#10599=DIRECTION('ref_axis',(0.,0.,-1.));
#10600=DIRECTION('center_axis',(0.,1.,0.));
#10601=DIRECTION('ref_axis',(1.,0.,0.));
#10602=DIRECTION('center_axis',(0.,-1.,0.));
#10603=DIRECTION('ref_axis',(1.,0.,0.));
#10604=DIRECTION('center_axis',(0.,-1.,0.));
#10605=DIRECTION('ref_axis',(1.,0.,0.));
#10606=DIRECTION('center_axis',(0.,-1.,0.));
#10607=DIRECTION('ref_axis',(0.,0.,-1.));
#10608=DIRECTION('center_axis',(0.,0.,1.));
#10609=DIRECTION('ref_axis',(1.,0.,0.));
#10610=DIRECTION('center_axis',(0.,-1.,0.));
#10611=DIRECTION('ref_axis',(0.,0.,-1.));
#10612=DIRECTION('center_axis',(0.,1.,0.));
#10613=DIRECTION('ref_axis',(1.,0.,0.));
#10614=DIRECTION('center_axis',(0.,-1.,0.));
#10615=DIRECTION('ref_axis',(1.,0.,0.));
#10616=DIRECTION('center_axis',(0.,-1.,0.));
#10617=DIRECTION('ref_axis',(0.,0.,-1.));
#10618=DIRECTION('center_axis',(8.96625347776458E-17,0.,1.));
#10619=DIRECTION('ref_axis',(1.,0.,0.));
#10620=DIRECTION('center_axis',(0.,-1.,0.));
#10621=DIRECTION('ref_axis',(0.,0.,-1.));
#10622=DIRECTION('center_axis',(0.,1.,0.));
#10623=DIRECTION('ref_axis',(1.,0.,0.));
#10624=DIRECTION('center_axis',(0.,-1.,0.));
#10625=DIRECTION('ref_axis',(1.,0.,0.));
#10626=DIRECTION('center_axis',(0.,-1.,0.));
#10627=DIRECTION('ref_axis',(0.,0.,-1.));
#10628=DIRECTION('center_axis',(0.,0.,1.));
#10629=DIRECTION('ref_axis',(1.,0.,0.));
#10630=DIRECTION('center_axis',(0.,-1.,0.));
#10631=DIRECTION('ref_axis',(0.,0.,-1.));
#10632=DIRECTION('center_axis',(0.,1.,0.));
#10633=DIRECTION('ref_axis',(1.,0.,0.));
#10634=DIRECTION('center_axis',(0.,1.,0.));
#10635=DIRECTION('ref_axis',(1.,0.,0.));
#10636=DIRECTION('',(0.,1.,0.));
#10637=DIRECTION('center_axis',(0.,-1.,0.));
#10638=DIRECTION('ref_axis',(1.,0.,0.));
#10639=DIRECTION('center_axis',(0.,-1.,0.));
#10640=DIRECTION('ref_axis',(1.,0.,0.));
#10641=DIRECTION('center_axis',(0.,1.,0.));
#10642=DIRECTION('ref_axis',(1.,0.,0.));
#10643=DIRECTION('center_axis',(0.,-1.,0.));
#10644=DIRECTION('ref_axis',(0.,0.,-1.));
#10645=DIRECTION('center_axis',(0.,0.,1.));
#10646=DIRECTION('ref_axis',(1.,0.,0.));
#10647=DIRECTION('center_axis',(0.,-1.,0.));
#10648=DIRECTION('ref_axis',(0.,0.,-1.));
#10649=DIRECTION('center_axis',(0.,-1.,0.));
#10650=DIRECTION('ref_axis',(-1.,0.,0.));
#10651=DIRECTION('center_axis',(0.,1.,0.));
#10652=DIRECTION('ref_axis',(1.,0.,0.));
#10653=DIRECTION('axis',(0.,0.,1.));
#10654=DIRECTION('refdir',(1.,0.,0.));
#10655=DIRECTION('center_axis',(0.,1.,0.));
#10656=DIRECTION('ref_axis',(0.,0.,1.));
#10657=DIRECTION('center_axis',(0.,-1.,0.));
#10658=DIRECTION('ref_axis',(1.,0.,0.));
#10659=DIRECTION('center_axis',(0.,-1.,0.));
#10660=DIRECTION('ref_axis',(1.,0.,0.));
#10661=DIRECTION('center_axis',(0.,-1.,0.));
#10662=DIRECTION('ref_axis',(1.,0.,0.));
#10663=DIRECTION('center_axis',(0.,-1.,0.));
#10664=DIRECTION('ref_axis',(1.,0.,0.));
#10665=DIRECTION('',(0.,1.,0.));
#10666=DIRECTION('center_axis',(0.,-1.,0.));
#10667=DIRECTION('ref_axis',(0.,0.,-1.));
#10668=DIRECTION('center_axis',(0.,-1.,0.));
#10669=DIRECTION('ref_axis',(1.,0.,0.));
#10670=DIRECTION('center_axis',(0.,-1.,0.));
#10671=DIRECTION('ref_axis',(1.,0.,0.));
#10672=DIRECTION('',(0.,1.,0.));
#10673=DIRECTION('center_axis',(0.,1.,0.));
#10674=DIRECTION('ref_axis',(0.,0.,1.));
#10675=DIRECTION('center_axis',(0.,-1.,0.));
#10676=DIRECTION('ref_axis',(1.,0.,0.));
#10677=DIRECTION('center_axis',(0.,-1.,0.));
#10678=DIRECTION('ref_axis',(1.,0.,0.));
#10679=DIRECTION('center_axis',(0.,-1.,0.));
#10680=DIRECTION('ref_axis',(1.,0.,0.));
#10681=DIRECTION('center_axis',(0.,-1.,0.));
#10682=DIRECTION('ref_axis',(1.,0.,0.));
#10683=DIRECTION('',(0.,1.,0.));
#10684=DIRECTION('center_axis',(0.,-1.,0.));
#10685=DIRECTION('ref_axis',(0.,0.,-1.));
#10686=DIRECTION('center_axis',(0.,-1.,0.));
#10687=DIRECTION('ref_axis',(1.,0.,0.));
#10688=DIRECTION('center_axis',(0.,-1.,0.));
#10689=DIRECTION('ref_axis',(1.,0.,0.));
#10690=DIRECTION('',(0.,1.,0.));
#10691=DIRECTION('',(0.,0.,1.));
#10692=DIRECTION('',(1.,0.,0.));
#10693=DIRECTION('',(0.,0.,1.));
#10694=DIRECTION('',(1.,0.,0.));
#10695=DIRECTION('',(0.,0.,1.));
#10696=DIRECTION('',(1.,0.,0.));
#10697=DIRECTION('',(0.,0.,1.));
#10698=DIRECTION('',(1.,0.,0.));
#10699=DIRECTION('',(0.,0.,1.));
#10700=DIRECTION('',(1.,0.,0.));
#10701=DIRECTION('axis',(0.,0.,1.));
#10702=DIRECTION('refdir',(1.,0.,0.));
#10703=DIRECTION('axis',(0.,0.,1.));
#10704=DIRECTION('refdir',(1.,0.,0.));
#10705=DIRECTION('center_axis',(0.,-1.,0.));
#10706=DIRECTION('ref_axis',(0.,0.,-1.));
#10707=DIRECTION('center_axis',(0.,-1.,0.));
#10708=DIRECTION('ref_axis',(1.,0.,0.));
#10709=DIRECTION('center_axis',(0.,-1.,0.));
#10710=DIRECTION('ref_axis',(1.,0.,0.));
#10711=DIRECTION('center_axis',(1.,0.,1.22464679914735E-16));
#10712=DIRECTION('ref_axis',(-1.22464679914735E-16,0.,1.));
#10713=DIRECTION('center_axis',(0.,1.,0.));
#10714=DIRECTION('ref_axis',(1.,0.,0.));
#10715=DIRECTION('center_axis',(0.,1.,0.));
#10716=DIRECTION('ref_axis',(1.,0.,0.));
#10717=DIRECTION('center_axis',(0.,-1.,0.));
#10718=DIRECTION('ref_axis',(1.,0.,0.));
#10719=DIRECTION('',(0.,1.,0.));
#10720=DIRECTION('center_axis',(0.,-1.,0.));
#10721=DIRECTION('ref_axis',(1.,0.,0.));
#10722=DIRECTION('center_axis',(0.,-1.,0.));
#10723=DIRECTION('ref_axis',(1.,0.,0.));
#10724=DIRECTION('center_axis',(0.,-1.,0.));
#10725=DIRECTION('ref_axis',(1.,0.,0.));
#10726=DIRECTION('',(0.,1.,0.));
#10727=DIRECTION('center_axis',(0.,-1.,0.));
#10728=DIRECTION('ref_axis',(1.,0.,0.));
#10729=DIRECTION('center_axis',(0.,1.,0.));
#10730=DIRECTION('ref_axis',(1.,0.,0.));
#10731=DIRECTION('',(-0.707106781186548,0.707106781186547,-8.65956056235494E-17));
#10732=DIRECTION('center_axis',(0.,-1.,0.));
#10733=DIRECTION('ref_axis',(1.,0.,0.));
#10734=DIRECTION('center_axis',(0.,1.,0.));
#10735=DIRECTION('ref_axis',(0.,0.,1.));
#10736=DIRECTION('center_axis',(0.,-1.,0.));
#10737=DIRECTION('ref_axis',(1.,0.,0.));
#10738=DIRECTION('center_axis',(0.,-1.,0.));
#10739=DIRECTION('ref_axis',(1.,0.,0.));
#10740=DIRECTION('',(0.,1.,0.));
#10741=DIRECTION('center_axis',(0.,-1.,0.));
#10742=DIRECTION('ref_axis',(0.,0.,-1.));
#10743=DIRECTION('center_axis',(0.,-1.,0.));
#10744=DIRECTION('ref_axis',(1.,0.,0.));
#10745=DIRECTION('center_axis',(0.,-1.,0.));
#10746=DIRECTION('ref_axis',(1.,0.,0.));
#10747=DIRECTION('',(0.707106781186548,0.707106781186547,8.65956056235494E-17));
#10748=DIRECTION('axis',(0.,0.,1.));
#10749=DIRECTION('refdir',(1.,0.,0.));
#10750=DIRECTION('center_axis',(0.,-1.,0.));
#10751=DIRECTION('ref_axis',(0.,0.,-1.));
#10752=DIRECTION('center_axis',(0.,-1.,0.));
#10753=DIRECTION('ref_axis',(1.,0.,0.));
#10754=DIRECTION('center_axis',(0.,-1.,0.));
#10755=DIRECTION('ref_axis',(1.,0.,0.));
#10756=DIRECTION('center_axis',(1.,0.,1.22464679914735E-16));
#10757=DIRECTION('ref_axis',(-1.22464679914735E-16,0.,1.));
#10758=DIRECTION('center_axis',(0.,1.,0.));
#10759=DIRECTION('ref_axis',(1.,0.,0.));
#10760=DIRECTION('center_axis',(0.,1.,0.));
#10761=DIRECTION('ref_axis',(1.,0.,0.));
#10762=DIRECTION('center_axis',(0.,-1.,0.));
#10763=DIRECTION('ref_axis',(1.,0.,0.));
#10764=DIRECTION('center_axis',(0.,-1.,0.));
#10765=DIRECTION('ref_axis',(1.,0.,0.));
#10766=DIRECTION('',(0.,1.,0.));
#10767=DIRECTION('center_axis',(0.,1.,0.));
#10768=DIRECTION('ref_axis',(0.,0.,1.));
#10769=DIRECTION('center_axis',(0.,-1.,0.));
#10770=DIRECTION('ref_axis',(1.,0.,0.));
#10771=DIRECTION('center_axis',(0.,-1.,0.));
#10772=DIRECTION('ref_axis',(1.,0.,0.));
#10773=DIRECTION('center_axis',(0.,-1.,0.));
#10774=DIRECTION('ref_axis',(1.,0.,0.));
#10775=DIRECTION('center_axis',(0.,-1.,0.));
#10776=DIRECTION('ref_axis',(1.,0.,0.));
#10777=DIRECTION('',(0.707106781186548,0.707106781186547,8.65956056235494E-17));
#10778=DIRECTION('center_axis',(0.,-1.,0.));
#10779=DIRECTION('ref_axis',(1.,0.,0.));
#10780=DIRECTION('center_axis',(0.,-1.,0.));
#10781=DIRECTION('ref_axis',(1.,0.,0.));
#10782=DIRECTION('',(0.,1.,0.));
#10783=DIRECTION('center_axis',(0.,1.,0.));
#10784=DIRECTION('ref_axis',(1.,0.,0.));
#10785=DIRECTION('center_axis',(0.,-1.,0.));
#10786=DIRECTION('ref_axis',(1.,0.,0.));
#10787=DIRECTION('',(-0.707106781186548,0.707106781186547,-8.65956056235494E-17));
#10788=DIRECTION('center_axis',(0.,-1.,0.));
#10789=DIRECTION('ref_axis',(0.,0.,-1.));
#10790=DIRECTION('center_axis',(0.,-1.,0.));
#10791=DIRECTION('ref_axis',(1.,0.,0.));
#10792=DIRECTION('',(0.,1.,0.));
#10793=DIRECTION('axis',(0.,0.,1.));
#10794=DIRECTION('refdir',(1.,0.,0.));
#10795=DIRECTION('center_axis',(0.,0.,1.));
#10796=DIRECTION('ref_axis',(1.,0.,0.));
#10797=DIRECTION('center_axis',(1.22464679914735E-16,-1.,0.));
#10798=DIRECTION('ref_axis',(-1.,-1.22464679914735E-16,0.));
#10799=DIRECTION('center_axis',(0.707106781186548,0.,0.707106781186548));
#10800=DIRECTION('ref_axis',(0.707106781186548,0.,-0.707106781186548));
#10801=DIRECTION('center_axis',(8.65956056235493E-17,-1.,-8.65956056235493E-17));
#10802=DIRECTION('ref_axis',(-0.707106781186548,-1.22464679914735E-16,0.707106781186548));
#10803=DIRECTION('center_axis',(1.,0.,0.));
#10804=DIRECTION('ref_axis',(6.12323399573677E-17,0.,-1.));
#10805=DIRECTION('center_axis',(7.49879891330929E-33,-1.,-1.22464679914735E-16));
#10806=DIRECTION('ref_axis',(-6.12323399573677E-17,-1.22464679914735E-16,
1.));
#10807=DIRECTION('center_axis',(0.707106781186548,0.,-0.707106781186548));
#10808=DIRECTION('ref_axis',(-0.707106781186548,0.,-0.707106781186548));
#10809=DIRECTION('center_axis',(-8.65956056235493E-17,-1.,-8.65956056235493E-17));
#10810=DIRECTION('ref_axis',(0.707106781186548,-1.22464679914735E-16,0.707106781186548));
#10811=DIRECTION('center_axis',(0.,0.,-1.));
#10812=DIRECTION('ref_axis',(-1.,0.,-1.22464679914735E-16));
#10813=DIRECTION('center_axis',(-1.22464679914735E-16,-1.,-1.49975978266186E-32));
#10814=DIRECTION('ref_axis',(1.,-1.22464679914735E-16,1.22464679914735E-16));
#10815=DIRECTION('center_axis',(-0.707106781186548,0.,-0.707106781186548));
#10816=DIRECTION('ref_axis',(-0.707106781186548,0.,0.707106781186548));
#10817=DIRECTION('center_axis',(-8.65956056235493E-17,-1.,8.65956056235493E-17));
#10818=DIRECTION('ref_axis',(0.707106781186548,-1.22464679914735E-16,-0.707106781186548));
#10819=DIRECTION('center_axis',(-1.,0.,0.));
#10820=DIRECTION('ref_axis',(-1.83697019872103E-16,0.,1.));
#10821=DIRECTION('center_axis',(-2.24963967399279E-32,-1.,1.22464679914735E-16));
#10822=DIRECTION('ref_axis',(1.83697019872103E-16,-1.22464679914735E-16,
-1.));
#10823=DIRECTION('center_axis',(-0.707106781186548,0.,0.707106781186548));
#10824=DIRECTION('ref_axis',(0.707106781186548,0.,0.707106781186548));
#10825=DIRECTION('center_axis',(8.65956056235493E-17,-1.,8.65956056235494E-17));
#10826=DIRECTION('ref_axis',(-0.707106781186548,-1.22464679914735E-16,-0.707106781186548));
#10827=DIRECTION('axis',(0.,0.,1.));
#10828=DIRECTION('refdir',(1.,0.,0.));
#10829=DIRECTION('center_axis',(0.,0.,1.));
#10830=DIRECTION('ref_axis',(1.,0.,0.));
#10831=DIRECTION('center_axis',(0.,-1.,0.));
#10832=DIRECTION('ref_axis',(0.,0.,-1.));
#10833=DIRECTION('center_axis',(0.,-1.,0.));
#10834=DIRECTION('ref_axis',(0.,0.,-1.));
#10835=DIRECTION('center_axis',(0.,1.,0.));
#10836=DIRECTION('ref_axis',(1.,0.,0.));
#10837=DIRECTION('center_axis',(0.,1.,0.));
#10838=DIRECTION('ref_axis',(1.,0.,0.));
#10839=DIRECTION('center_axis',(0.,1.,0.));
#10840=DIRECTION('ref_axis',(1.,0.,0.));
#10841=DIRECTION('center_axis',(0.,1.,0.));
#10842=DIRECTION('ref_axis',(1.,0.,0.));
#10843=DIRECTION('',(0.,-1.,0.));
#10844=DIRECTION('center_axis',(0.,-1.,0.));
#10845=DIRECTION('ref_axis',(1.,0.,0.));
#10846=DIRECTION('center_axis',(0.,1.,0.));
#10847=DIRECTION('ref_axis',(1.,0.,0.));
#10848=DIRECTION('center_axis',(0.,1.,0.));
#10849=DIRECTION('ref_axis',(1.,0.,0.));
#10850=DIRECTION('center_axis',(0.,1.,0.));
#10851=DIRECTION('ref_axis',(1.,0.,0.));
#10852=DIRECTION('center_axis',(0.,1.,0.));
#10853=DIRECTION('ref_axis',(1.,0.,0.));
#10854=DIRECTION('center_axis',(0.,1.,0.));
#10855=DIRECTION('ref_axis',(1.,0.,0.));
#10856=DIRECTION('center_axis',(0.,1.,0.));
#10857=DIRECTION('ref_axis',(1.,0.,0.));
#10858=DIRECTION('center_axis',(0.,-1.,0.));
#10859=DIRECTION('ref_axis',(1.,0.,0.));
#10860=DIRECTION('center_axis',(0.,-1.,0.));
#10861=DIRECTION('ref_axis',(0.,0.,-1.));
#10862=DIRECTION('center_axis',(6.12323399573677E-17,0.,1.));
#10863=DIRECTION('ref_axis',(1.,0.,0.));
#10864=DIRECTION('center_axis',(0.,-1.,0.));
#10865=DIRECTION('ref_axis',(0.,0.,-1.));
#10866=DIRECTION('center_axis',(0.,1.,0.));
#10867=DIRECTION('ref_axis',(1.,0.,0.));
#10868=DIRECTION('center_axis',(0.,-1.,0.));
#10869=DIRECTION('ref_axis',(1.,0.,0.));
#10870=DIRECTION('center_axis',(0.,-1.,0.));
#10871=DIRECTION('ref_axis',(0.,0.,-1.));
#10872=DIRECTION('center_axis',(0.,0.,1.));
#10873=DIRECTION('ref_axis',(1.,0.,0.));
#10874=DIRECTION('center_axis',(0.,-1.,0.));
#10875=DIRECTION('ref_axis',(0.,0.,-1.));
#10876=DIRECTION('center_axis',(0.,1.,0.));
#10877=DIRECTION('ref_axis',(1.,0.,0.));
#10878=DIRECTION('center_axis',(0.,-1.,0.));
#10879=DIRECTION('ref_axis',(1.,0.,0.));
#10880=DIRECTION('center_axis',(0.,-1.,0.));
#10881=DIRECTION('ref_axis',(0.,0.,-1.));
#10882=DIRECTION('center_axis',(0.,0.,1.));
#10883=DIRECTION('ref_axis',(1.,0.,0.));
#10884=DIRECTION('center_axis',(0.,-1.,0.));
#10885=DIRECTION('ref_axis',(0.,0.,-1.));
#10886=DIRECTION('center_axis',(0.,1.,0.));
#10887=DIRECTION('ref_axis',(1.,0.,0.));
#10888=DIRECTION('center_axis',(0.,-1.,0.));
#10889=DIRECTION('ref_axis',(1.,0.,0.));
#10890=DIRECTION('center_axis',(0.,-1.,0.));
#10891=DIRECTION('ref_axis',(0.,0.,-1.));
#10892=DIRECTION('center_axis',(0.,0.,1.));
#10893=DIRECTION('ref_axis',(1.,0.,0.));
#10894=DIRECTION('center_axis',(0.,-1.,0.));
#10895=DIRECTION('ref_axis',(0.,0.,-1.));
#10896=DIRECTION('center_axis',(0.,1.,0.));
#10897=DIRECTION('ref_axis',(1.,0.,0.));
#10898=DIRECTION('center_axis',(0.,-1.,0.));
#10899=DIRECTION('ref_axis',(1.,0.,0.));
#10900=DIRECTION('center_axis',(0.,-1.,0.));
#10901=DIRECTION('ref_axis',(0.,0.,-1.));
#10902=DIRECTION('center_axis',(6.12323399573676E-17,0.,1.));
#10903=DIRECTION('ref_axis',(1.,0.,0.));
#10904=DIRECTION('center_axis',(0.,-1.,0.));
#10905=DIRECTION('ref_axis',(0.,0.,-1.));
#10906=DIRECTION('center_axis',(0.,1.,0.));
#10907=DIRECTION('ref_axis',(1.,0.,0.));
#10908=DIRECTION('center_axis',(0.,-1.,0.));
#10909=DIRECTION('ref_axis',(1.,0.,0.));
#10910=DIRECTION('center_axis',(0.,-1.,0.));
#10911=DIRECTION('ref_axis',(0.,0.,-1.));
#10912=DIRECTION('center_axis',(0.,0.,1.));
#10913=DIRECTION('ref_axis',(1.,0.,0.));
#10914=DIRECTION('center_axis',(0.,-1.,0.));
#10915=DIRECTION('ref_axis',(0.,0.,-1.));
#10916=DIRECTION('center_axis',(0.,1.,0.));
#10917=DIRECTION('ref_axis',(1.,0.,0.));
#10918=DIRECTION('center_axis',(0.,1.,0.));
#10919=DIRECTION('ref_axis',(1.,0.,0.));
#10920=DIRECTION('',(0.,1.,0.));
#10921=DIRECTION('center_axis',(0.,-1.,0.));
#10922=DIRECTION('ref_axis',(1.,0.,0.));
#10923=DIRECTION('center_axis',(0.,-1.,0.));
#10924=DIRECTION('ref_axis',(1.,0.,0.));
#10925=DIRECTION('center_axis',(0.,1.,0.));
#10926=DIRECTION('ref_axis',(1.,0.,0.));
#10927=DIRECTION('center_axis',(0.,-1.,0.));
#10928=DIRECTION('ref_axis',(0.,0.,-1.));
#10929=DIRECTION('center_axis',(0.,0.,1.));
#10930=DIRECTION('ref_axis',(1.,0.,0.));
#10931=DIRECTION('center_axis',(0.,-1.,0.));
#10932=DIRECTION('ref_axis',(0.,0.,-1.));
#10933=DIRECTION('center_axis',(0.,-1.,0.));
#10934=DIRECTION('ref_axis',(-1.,0.,0.));
#10935=DIRECTION('center_axis',(0.,1.,0.));
#10936=DIRECTION('ref_axis',(1.,0.,0.));
#10937=DIRECTION('axis',(0.,0.,1.));
#10938=DIRECTION('refdir',(1.,0.,0.));
#10939=DIRECTION('center_axis',(0.,1.,0.));
#10940=DIRECTION('ref_axis',(0.,0.,1.));
#10941=DIRECTION('center_axis',(0.,-1.,0.));
#10942=DIRECTION('ref_axis',(1.,0.,0.));
#10943=DIRECTION('center_axis',(0.,-1.,0.));
#10944=DIRECTION('ref_axis',(1.,0.,0.));
#10945=DIRECTION('center_axis',(0.,-1.,0.));
#10946=DIRECTION('ref_axis',(1.,0.,0.));
#10947=DIRECTION('center_axis',(0.,-1.,0.));
#10948=DIRECTION('ref_axis',(1.,0.,0.));
#10949=DIRECTION('',(0.,1.,0.));
#10950=DIRECTION('center_axis',(0.,-1.,0.));
#10951=DIRECTION('ref_axis',(0.,0.,-1.));
#10952=DIRECTION('center_axis',(0.,-1.,0.));
#10953=DIRECTION('ref_axis',(1.,0.,0.));
#10954=DIRECTION('center_axis',(0.,-1.,0.));
#10955=DIRECTION('ref_axis',(1.,0.,0.));
#10956=DIRECTION('',(0.,1.,0.));
#10957=DIRECTION('center_axis',(0.,1.,0.));
#10958=DIRECTION('ref_axis',(0.,0.,1.));
#10959=DIRECTION('center_axis',(0.,-1.,0.));
#10960=DIRECTION('ref_axis',(1.,0.,0.));
#10961=DIRECTION('center_axis',(0.,-1.,0.));
#10962=DIRECTION('ref_axis',(1.,0.,0.));
#10963=DIRECTION('center_axis',(0.,-1.,0.));
#10964=DIRECTION('ref_axis',(1.,0.,0.));
#10965=DIRECTION('center_axis',(0.,-1.,0.));
#10966=DIRECTION('ref_axis',(1.,0.,0.));
#10967=DIRECTION('',(0.,1.,0.));
#10968=DIRECTION('center_axis',(0.,-1.,0.));
#10969=DIRECTION('ref_axis',(0.,0.,-1.));
#10970=DIRECTION('center_axis',(0.,-1.,0.));
#10971=DIRECTION('ref_axis',(1.,0.,0.));
#10972=DIRECTION('center_axis',(0.,-1.,0.));
#10973=DIRECTION('ref_axis',(1.,0.,0.));
#10974=DIRECTION('',(0.,1.,0.));
#10975=DIRECTION('',(0.,0.,1.));
#10976=DIRECTION('',(1.,0.,0.));
#10977=DIRECTION('',(0.,0.,1.));
#10978=DIRECTION('',(1.,0.,0.));
#10979=DIRECTION('',(0.,0.,1.));
#10980=DIRECTION('',(1.,0.,0.));
#10981=DIRECTION('',(0.,0.,1.));
#10982=DIRECTION('',(1.,0.,0.));
#10983=DIRECTION('',(0.,0.,1.));
#10984=DIRECTION('',(1.,0.,0.));
#10985=DIRECTION('axis',(0.,0.,1.));
#10986=DIRECTION('refdir',(1.,0.,0.));
#10987=DIRECTION('center_axis',(0.,1.,0.));
#10988=DIRECTION('ref_axis',(0.,0.,1.));
#10989=DIRECTION('center_axis',(0.,-1.,0.));
#10990=DIRECTION('ref_axis',(1.,0.,0.));
#10991=DIRECTION('center_axis',(0.,-1.,0.));
#10992=DIRECTION('ref_axis',(1.,0.,0.));
#10993=DIRECTION('center_axis',(0.,-1.,0.));
#10994=DIRECTION('ref_axis',(1.,0.,0.));
#10995=DIRECTION('',(0.707106781186548,0.707106781186547,8.65956056235493E-17));
#10996=DIRECTION('center_axis',(0.,-1.,0.));
#10997=DIRECTION('ref_axis',(1.,0.,0.));
#10998=DIRECTION('center_axis',(0.,-1.,0.));
#10999=DIRECTION('ref_axis',(1.,0.,0.));
#11000=DIRECTION('',(0.,1.,0.));
#11001=DIRECTION('center_axis',(0.,1.,0.));
#11002=DIRECTION('ref_axis',(1.,0.,0.));
#11003=DIRECTION('center_axis',(0.,-1.,0.));
#11004=DIRECTION('ref_axis',(1.,0.,0.));
#11005=DIRECTION('',(-0.707106781186547,0.707106781186548,-8.65956056235493E-17));
#11006=DIRECTION('center_axis',(0.,-1.,0.));
#11007=DIRECTION('ref_axis',(0.,0.,-1.));
#11008=DIRECTION('center_axis',(0.,-1.,0.));
#11009=DIRECTION('ref_axis',(1.,0.,0.));
#11010=DIRECTION('center_axis',(0.,1.,0.));
#11011=DIRECTION('ref_axis',(1.,0.,0.));
#11012=DIRECTION('center_axis',(0.,1.,0.));
#11013=DIRECTION('ref_axis',(1.,0.,0.));
#11014=DIRECTION('',(-0.447213595499958,0.894427190999916,-5.47678698264203E-17));
#11015=DIRECTION('center_axis',(0.,-1.,0.));
#11016=DIRECTION('ref_axis',(1.,0.,0.));
#11017=DIRECTION('center_axis',(0.,1.,0.));
#11018=DIRECTION('ref_axis',(1.,0.,0.));
#11019=DIRECTION('',(0.,1.,0.));
#11020=DIRECTION('center_axis',(0.,1.,0.));
#11021=DIRECTION('ref_axis',(1.,0.,0.));
#11022=DIRECTION('center_axis',(0.,-1.,0.));
#11023=DIRECTION('ref_axis',(1.,0.,0.));
#11024=DIRECTION('',(-0.707106781186547,0.707106781186548,-8.65956056235493E-17));
#11025=DIRECTION('center_axis',(0.,-1.,0.));
#11026=DIRECTION('ref_axis',(0.,0.,-1.));
#11027=DIRECTION('center_axis',(0.866025403784439,0.,-0.5));
#11028=DIRECTION('ref_axis',(0.5,0.,0.866025403784439));
#11029=DIRECTION('',(-0.5,0.,-0.866025403784439));
#11030=DIRECTION('',(0.,-1.,0.));
#11031=DIRECTION('',(0.5,0.,0.866025403784439));
#11032=DIRECTION('',(0.,-1.,0.));
#11033=DIRECTION('center_axis',(1.20185167898973E-16,0.,-1.));
#11034=DIRECTION('ref_axis',(1.,0.,1.20185167898973E-16));
#11035=DIRECTION('',(-1.,0.,-1.20185167898973E-16));
#11036=DIRECTION('',(0.,-1.,0.));
#11037=DIRECTION('',(1.,0.,1.20185167898973E-16));
#11038=DIRECTION('center_axis',(-0.866025403784439,0.,-0.5));
#11039=DIRECTION('ref_axis',(0.5,0.,-0.866025403784439));
#11040=DIRECTION('',(-0.5,0.,0.866025403784439));
#11041=DIRECTION('',(0.,-1.,0.));
#11042=DIRECTION('',(0.5,0.,-0.866025403784439));
#11043=DIRECTION('center_axis',(-0.866025403784439,0.,0.5));
#11044=DIRECTION('ref_axis',(-0.5,0.,-0.866025403784439));
#11045=DIRECTION('',(0.5,0.,0.866025403784439));
#11046=DIRECTION('',(0.,-1.,0.));
#11047=DIRECTION('',(-0.5,0.,-0.866025403784439));
#11048=DIRECTION('center_axis',(-2.40370335797945E-16,0.,1.));
#11049=DIRECTION('ref_axis',(-1.,0.,-2.40370335797945E-16));
#11050=DIRECTION('',(1.,0.,2.40370335797945E-16));
#11051=DIRECTION('',(0.,-1.,0.));
#11052=DIRECTION('',(-1.,0.,-2.40370335797945E-16));
#11053=DIRECTION('center_axis',(0.866025403784439,0.,0.5));
#11054=DIRECTION('ref_axis',(-0.5,0.,0.866025403784439));
#11055=DIRECTION('',(0.5,0.,-0.866025403784439));
#11056=DIRECTION('',(-0.5,0.,0.866025403784439));
#11057=DIRECTION('center_axis',(0.,1.,0.));
#11058=DIRECTION('ref_axis',(1.,0.,0.));
#11059=DIRECTION('center_axis',(0.,-1.,0.));
#11060=DIRECTION('ref_axis',(0.,0.,-1.));
#11061=DIRECTION('axis',(0.,0.,1.));
#11062=DIRECTION('refdir',(1.,0.,0.));
#11063=DIRECTION('center_axis',(0.866025403784439,0.,-0.5));
#11064=DIRECTION('ref_axis',(0.5,0.,0.866025403784439));
#11065=DIRECTION('',(-0.5,0.,-0.866025403784439));
#11066=DIRECTION('',(0.,-1.,0.));
#11067=DIRECTION('',(0.5,0.,0.866025403784439));
#11068=DIRECTION('',(0.,-1.,0.));
#11069=DIRECTION('center_axis',(1.60246890531964E-16,0.,-1.));
#11070=DIRECTION('ref_axis',(1.,0.,1.60246890531964E-16));
#11071=DIRECTION('',(-1.,0.,-1.60246890531964E-16));
#11072=DIRECTION('',(0.,-1.,0.));
#11073=DIRECTION('',(1.,0.,1.60246890531964E-16));
#11074=DIRECTION('center_axis',(-0.866025403784439,0.,-0.5));
#11075=DIRECTION('ref_axis',(0.5,0.,-0.866025403784439));
#11076=DIRECTION('',(-0.5,0.,0.866025403784439));
#11077=DIRECTION('',(0.,-1.,0.));
#11078=DIRECTION('',(0.5,0.,-0.866025403784439));
#11079=DIRECTION('center_axis',(-0.866025403784439,0.,0.5));
#11080=DIRECTION('ref_axis',(-0.5,0.,-0.866025403784439));
#11081=DIRECTION('',(0.5,0.,0.866025403784439));
#11082=DIRECTION('',(0.,-1.,0.));
#11083=DIRECTION('',(-0.5,0.,-0.866025403784439));
#11084=DIRECTION('center_axis',(-1.60246890531964E-16,0.,1.));
#11085=DIRECTION('ref_axis',(-1.,0.,-1.60246890531964E-16));
#11086=DIRECTION('',(1.,0.,1.60246890531964E-16));
#11087=DIRECTION('',(0.,-1.,0.));
#11088=DIRECTION('',(-1.,0.,-1.60246890531964E-16));
#11089=DIRECTION('center_axis',(0.866025403784439,0.,0.5));
#11090=DIRECTION('ref_axis',(-0.5,0.,0.866025403784439));
#11091=DIRECTION('',(0.5,0.,-0.866025403784439));
#11092=DIRECTION('',(-0.5,0.,0.866025403784439));
#11093=DIRECTION('center_axis',(0.,1.,0.));
#11094=DIRECTION('ref_axis',(1.,0.,0.));
#11095=DIRECTION('center_axis',(0.,-1.,0.));
#11096=DIRECTION('ref_axis',(0.,0.,-1.));
#11097=DIRECTION('center_axis',(0.,1.,0.));
#11098=DIRECTION('ref_axis',(1.,0.,0.));
#11099=DIRECTION('center_axis',(0.,1.,0.));
#11100=DIRECTION('ref_axis',(1.,0.,0.));
#11101=DIRECTION('center_axis',(0.,1.,0.));
#11102=DIRECTION('ref_axis',(0.,0.,1.));
#11103=DIRECTION('center_axis',(0.,-1.,0.));
#11104=DIRECTION('ref_axis',(1.,0.,0.));
#11105=DIRECTION('center_axis',(0.,-1.,0.));
#11106=DIRECTION('ref_axis',(1.,0.,0.));
#11107=DIRECTION('center_axis',(0.,-1.,0.));
#11108=DIRECTION('ref_axis',(1.,0.,0.));
#11109=DIRECTION('',(0.707106781186547,0.707106781186548,8.65956056235493E-17));
#11110=DIRECTION('center_axis',(0.,-1.,0.));
#11111=DIRECTION('ref_axis',(1.,0.,0.));
#11112=DIRECTION('center_axis',(0.,-1.,0.));
#11113=DIRECTION('ref_axis',(1.,0.,0.));
#11114=DIRECTION('',(0.,1.,0.));
#11115=DIRECTION('center_axis',(0.,1.,0.));
#11116=DIRECTION('ref_axis',(1.,0.,0.));
#11117=DIRECTION('center_axis',(0.,-1.,0.));
#11118=DIRECTION('ref_axis',(1.,0.,0.));
#11119=DIRECTION('',(-0.707106781186547,0.707106781186548,-8.65956056235493E-17));
#11120=DIRECTION('center_axis',(0.,-1.,0.));
#11121=DIRECTION('ref_axis',(0.,0.,-1.));
#11122=DIRECTION('center_axis',(0.,-1.,0.));
#11123=DIRECTION('ref_axis',(1.,0.,0.));
#11124=DIRECTION('center_axis',(0.,1.,0.));
#11125=DIRECTION('ref_axis',(1.,0.,0.));
#11126=DIRECTION('center_axis',(0.,1.,0.));
#11127=DIRECTION('ref_axis',(1.,0.,0.));
#11128=DIRECTION('',(-0.447213595499958,0.894427190999916,-5.47678698264203E-17));
#11129=DIRECTION('center_axis',(0.,-1.,0.));
#11130=DIRECTION('ref_axis',(1.,0.,0.));
#11131=DIRECTION('',(0.,1.,0.));
#11132=DIRECTION('',(0.,0.,1.));
#11133=DIRECTION('',(1.,0.,0.));
#11134=DIRECTION('',(0.,0.,1.));
#11135=DIRECTION('',(1.,0.,0.));
#11136=DIRECTION('',(0.,0.,1.));
#11137=DIRECTION('',(1.,0.,0.));
#11138=DIRECTION('',(0.,0.,1.));
#11139=DIRECTION('',(1.,0.,0.));
#11140=DIRECTION('',(0.,0.,1.));
#11141=DIRECTION('',(1.,0.,0.));
#11142=DIRECTION('',(0.,0.,1.));
#11143=DIRECTION('',(1.,0.,0.));
#11144=DIRECTION('',(0.,0.,1.));
#11145=DIRECTION('',(1.,0.,0.));
#11146=DIRECTION('',(0.,0.,1.));
#11147=DIRECTION('',(1.,0.,0.));
#11148=DIRECTION('',(0.,0.,1.));
#11149=DIRECTION('',(1.,0.,0.));
#11150=DIRECTION('',(0.,0.,1.));
#11151=DIRECTION('',(1.,0.,0.));
#11152=DIRECTION('',(0.,0.,1.));
#11153=DIRECTION('',(1.,0.,0.));
#11154=DIRECTION('',(0.,0.,1.));
#11155=DIRECTION('',(1.,0.,0.));
#11156=DIRECTION('',(0.,0.,1.));
#11157=DIRECTION('',(1.,0.,0.));
#11158=DIRECTION('',(0.,0.,1.));
#11159=DIRECTION('',(1.,0.,0.));
#11160=DIRECTION('',(0.,0.,1.));
#11161=DIRECTION('',(1.,0.,0.));
#11162=DIRECTION('',(0.,-1.,2.22044604925031E-16));
#11163=DIRECTION('',(1.,0.,0.));
#11164=DIRECTION('',(0.,-1.,2.22044604925031E-16));
#11165=DIRECTION('',(1.,0.,0.));
#11166=DIRECTION('',(0.,0.,1.));
#11167=DIRECTION('',(1.,0.,0.));
#11168=DIRECTION('',(0.,0.,1.));
#11169=DIRECTION('',(-1.,1.22464679914735E-16,0.));
#11170=DIRECTION('',(0.,0.,1.));
#11171=DIRECTION('',(-1.,1.22464679914735E-16,0.));
#11172=DIRECTION('',(0.,0.,1.));
#11173=DIRECTION('',(-1.,1.22464679914735E-16,0.));
#11174=DIRECTION('',(0.,0.,1.));
#11175=DIRECTION('',(-1.,1.22464679914735E-16,0.));
#11176=DIRECTION('',(0.,0.,1.));
#11177=DIRECTION('',(1.,0.,0.));
#11178=DIRECTION('',(0.,0.,1.));
#11179=DIRECTION('',(1.,0.,0.));
#11180=DIRECTION('',(0.,0.,1.));
#11181=DIRECTION('',(1.,0.,0.));
#11182=DIRECTION('',(0.,0.,1.));
#11183=DIRECTION('',(1.,0.,0.));
#11184=DIRECTION('',(0.,-1.,2.22044604925031E-16));
#11185=DIRECTION('',(1.,0.,0.));
#11186=DIRECTION('',(0.,-1.,2.22044604925031E-16));
#11187=DIRECTION('',(1.,0.,0.));
#11188=DIRECTION('',(0.,0.,1.));
#11189=DIRECTION('',(1.,0.,0.));
#11190=DIRECTION('',(0.,0.,1.));
#11191=DIRECTION('',(-1.,1.22464679914735E-16,0.));
#11192=DIRECTION('',(0.,0.,1.));
#11193=DIRECTION('',(-1.,1.22464679914735E-16,0.));
#11194=DIRECTION('',(0.,0.,1.));
#11195=DIRECTION('',(-1.,1.22464679914735E-16,0.));
#11196=DIRECTION('',(0.,0.,1.));
#11197=DIRECTION('',(-1.,1.22464679914735E-16,0.));
#11198=DIRECTION('',(0.,0.,1.));
#11199=DIRECTION('',(1.,0.,0.));
#11200=DIRECTION('',(0.,0.,1.));
#11201=DIRECTION('',(1.,0.,0.));
#11202=DIRECTION('',(0.,0.,1.));
#11203=DIRECTION('',(1.,0.,0.));
#11204=DIRECTION('',(0.,0.,1.));
#11205=DIRECTION('',(1.,0.,0.));
#11206=DIRECTION('',(0.,0.,1.));
#11207=DIRECTION('',(1.,0.,0.));
#11208=DIRECTION('',(0.,0.,1.));
#11209=DIRECTION('',(-1.,1.22464679914735E-16,0.));
#11210=DIRECTION('',(0.,0.,1.));
#11211=DIRECTION('',(-1.,1.22464679914735E-16,0.));
#11212=DIRECTION('',(0.,0.,1.));
#11213=DIRECTION('',(-1.,1.22464679914735E-16,0.));
#11214=DIRECTION('',(0.,0.,1.));
#11215=DIRECTION('',(-1.,1.22464679914735E-16,0.));
#11216=DIRECTION('',(0.,0.,1.));
#11217=DIRECTION('',(1.,0.,0.));
#11218=DIRECTION('',(0.,0.,1.));
#11219=DIRECTION('',(1.,0.,0.));
#11220=DIRECTION('',(0.,0.,1.));
#11221=DIRECTION('',(1.,0.,0.));
#11222=DIRECTION('',(0.,0.,1.));
#11223=DIRECTION('',(1.,0.,0.));
#11224=DIRECTION('',(0.,-1.,2.22044604925031E-16));
#11225=DIRECTION('',(1.,0.,0.));
#11226=DIRECTION('',(0.,-1.,2.22044604925031E-16));
#11227=DIRECTION('',(1.,0.,0.));
#11228=DIRECTION('',(0.,-1.,2.22044604925031E-16));
#11229=DIRECTION('',(1.,0.,0.));
#11230=DIRECTION('',(0.,-1.,2.22044604925031E-16));
#11231=DIRECTION('',(1.,0.,0.));
#11232=DIRECTION('',(0.,-1.,2.22044604925031E-16));
#11233=DIRECTION('',(1.,0.,0.));
#11234=DIRECTION('',(0.,-1.,2.22044604925031E-16));
#11235=DIRECTION('',(1.,0.,0.));
#11236=DIRECTION('',(0.,-1.,2.22044604925031E-16));
#11237=DIRECTION('',(1.,0.,0.));
#11238=DIRECTION('',(0.,-1.,2.22044604925031E-16));
#11239=DIRECTION('',(1.,0.,0.));
#11240=DIRECTION('',(0.,-1.,2.22044604925031E-16));
#11241=DIRECTION('',(1.,0.,0.));
#11242=DIRECTION('',(0.,-1.,2.22044604925031E-16));
#11243=DIRECTION('',(1.,0.,0.));
#11244=DIRECTION('axis',(0.,0.,1.));
#11245=DIRECTION('refdir',(1.,0.,0.));
#11246=DIRECTION('axis',(0.,0.,1.));
#11247=DIRECTION('refdir',(1.,0.,0.));
#11248=DIRECTION('center_axis',(0.,1.,0.));
#11249=DIRECTION('ref_axis',(1.,0.,0.));
#11250=DIRECTION('center_axis',(0.,1.,0.));
#11251=DIRECTION('ref_axis',(1.,0.,0.));
#11252=DIRECTION('',(0.,-1.,0.));
#11253=DIRECTION('center_axis',(0.,-1.,0.));
#11254=DIRECTION('ref_axis',(1.,0.,0.));
#11255=DIRECTION('center_axis',(0.,1.,0.));
#11256=DIRECTION('ref_axis',(1.,0.,0.));
#11257=DIRECTION('center_axis',(0.,1.,0.));
#11258=DIRECTION('ref_axis',(1.,0.,0.));
#11259=DIRECTION('center_axis',(0.,1.,0.));
#11260=DIRECTION('ref_axis',(1.,0.,0.));
#11261=DIRECTION('',(0.,-1.,0.));
#11262=DIRECTION('center_axis',(0.,1.,0.));
#11263=DIRECTION('ref_axis',(1.,0.,0.));
#11264=DIRECTION('center_axis',(0.,1.,0.));
#11265=DIRECTION('ref_axis',(1.,0.,0.));
#11266=DIRECTION('center_axis',(0.,1.,0.));
#11267=DIRECTION('ref_axis',(1.,0.,0.));
#11268=DIRECTION('center_axis',(0.,1.,0.));
#11269=DIRECTION('ref_axis',(1.,0.,0.));
#11270=DIRECTION('',(0.,-1.,0.));
#11271=DIRECTION('center_axis',(0.,1.,0.));
#11272=DIRECTION('ref_axis',(1.,0.,0.));
#11273=DIRECTION('center_axis',(0.,1.,0.));
#11274=DIRECTION('ref_axis',(1.,0.,0.));
#11275=DIRECTION('center_axis',(0.,1.,0.));
#11276=DIRECTION('ref_axis',(1.,0.,0.));
#11277=DIRECTION('axis',(0.,0.,1.));
#11278=DIRECTION('refdir',(1.,0.,0.));
#11279=DIRECTION('center_axis',(0.,1.,0.));
#11280=DIRECTION('ref_axis',(1.,0.,0.));
#11281=DIRECTION('center_axis',(0.,-1.,0.));
#11282=DIRECTION('ref_axis',(1.,0.,0.));
#11283=DIRECTION('',(0.,-1.,0.));
#11284=DIRECTION('center_axis',(0.,-1.,0.));
#11285=DIRECTION('ref_axis',(1.,0.,0.));
#11286=DIRECTION('center_axis',(0.,1.,0.));
#11287=DIRECTION('ref_axis',(1.,0.,0.));
#11288=DIRECTION('center_axis',(0.,1.,0.));
#11289=DIRECTION('ref_axis',(1.,0.,0.));
#11290=DIRECTION('',(0.,-1.,0.));
#11291=DIRECTION('center_axis',(0.,1.,0.));
#11292=DIRECTION('ref_axis',(1.,0.,0.));
#11293=DIRECTION('center_axis',(0.,1.,0.));
#11294=DIRECTION('ref_axis',(1.,0.,0.));
#11295=DIRECTION('center_axis',(0.,1.,0.));
#11296=DIRECTION('ref_axis',(1.,0.,0.));
#11297=DIRECTION('axis',(0.,0.,1.));
#11298=DIRECTION('refdir',(1.,0.,0.));
#11299=DIRECTION('center_axis',(0.,1.,0.));
#11300=DIRECTION('ref_axis',(1.,0.,0.));
#11301=DIRECTION('center_axis',(0.,-1.,0.));
#11302=DIRECTION('ref_axis',(1.,0.,0.));
#11303=DIRECTION('',(0.,-1.,0.));
#11304=DIRECTION('center_axis',(0.,-1.,0.));
#11305=DIRECTION('ref_axis',(1.,0.,0.));
#11306=DIRECTION('center_axis',(0.,1.,0.));
#11307=DIRECTION('ref_axis',(1.,0.,0.));
#11308=DIRECTION('center_axis',(0.,1.,0.));
#11309=DIRECTION('ref_axis',(1.,0.,0.));
#11310=DIRECTION('',(0.,-1.,0.));
#11311=DIRECTION('center_axis',(0.,1.,0.));
#11312=DIRECTION('ref_axis',(1.,0.,0.));
#11313=DIRECTION('center_axis',(0.,1.,0.));
#11314=DIRECTION('ref_axis',(1.,0.,0.));
#11315=DIRECTION('center_axis',(0.,1.,0.));
#11316=DIRECTION('ref_axis',(1.,0.,0.));
#11317=DIRECTION('axis',(0.,0.,1.));
#11318=DIRECTION('refdir',(1.,0.,0.));
#11319=DIRECTION('center_axis',(0.,0.,1.));
#11320=DIRECTION('ref_axis',(1.,0.,0.));
#11321=DIRECTION('',(0.,1.,0.));
#11322=DIRECTION('center_axis',(0.,0.,1.));
#11323=DIRECTION('ref_axis',(1.,0.,0.));
#11324=DIRECTION('center_axis',(0.,0.,1.));
#11325=DIRECTION('ref_axis',(1.,0.,0.));
#11326=DIRECTION('center_axis',(0.,0.,1.));
#11327=DIRECTION('ref_axis',(1.,0.,0.));
#11328=DIRECTION('',(0.,0.,1.));
#11329=DIRECTION('center_axis',(0.,0.,1.));
#11330=DIRECTION('ref_axis',(1.,0.,0.));
#11331=DIRECTION('center_axis',(0.,0.,1.));
#11332=DIRECTION('ref_axis',(1.,0.,0.));
#11333=DIRECTION('',(0.,-1.,0.));
#11334=DIRECTION('center_axis',(0.,1.,0.));
#11335=DIRECTION('ref_axis',(1.,0.,0.));
#11336=DIRECTION('center_axis',(0.,-1.,0.));
#11337=DIRECTION('ref_axis',(1.,0.,0.));
#11338=DIRECTION('',(0.,-1.,0.));
#11339=DIRECTION('center_axis',(0.,-1.,0.));
#11340=DIRECTION('ref_axis',(1.,0.,0.));
#11341=DIRECTION('center_axis',(0.,1.,0.));
#11342=DIRECTION('ref_axis',(1.,0.,0.));
#11343=DIRECTION('center_axis',(0.,1.,0.));
#11344=DIRECTION('ref_axis',(1.,0.,0.));
#11345=DIRECTION('',(0.,-1.,0.));
#11346=DIRECTION('center_axis',(0.,1.,0.));
#11347=DIRECTION('ref_axis',(1.,0.,0.));
#11348=DIRECTION('center_axis',(0.,1.,0.));
#11349=DIRECTION('ref_axis',(1.,0.,0.));
#11350=DIRECTION('center_axis',(0.,1.,0.));
#11351=DIRECTION('ref_axis',(1.,0.,0.));
#11352=DIRECTION('axis',(0.,0.,1.));
#11353=DIRECTION('refdir',(1.,0.,0.));
#11354=DIRECTION('center_axis',(0.,0.,1.));
#11355=DIRECTION('ref_axis',(1.,0.,0.));
#11356=DIRECTION('',(0.,1.,0.));
#11357=DIRECTION('center_axis',(0.,0.,1.));
#11358=DIRECTION('ref_axis',(1.,0.,0.));
#11359=DIRECTION('center_axis',(0.,0.,1.));
#11360=DIRECTION('ref_axis',(1.,0.,0.));
#11361=DIRECTION('center_axis',(0.,0.,1.));
#11362=DIRECTION('ref_axis',(1.,0.,0.));
#11363=DIRECTION('',(0.,0.,1.));
#11364=DIRECTION('center_axis',(0.,0.,1.));
#11365=DIRECTION('ref_axis',(1.,0.,0.));
#11366=DIRECTION('center_axis',(0.,0.,1.));
#11367=DIRECTION('ref_axis',(1.,0.,0.));
#11368=DIRECTION('',(0.,-1.,0.));
#11369=DIRECTION('center_axis',(0.,1.,0.));
#11370=DIRECTION('ref_axis',(1.,0.,0.));
#11371=DIRECTION('center_axis',(0.,-1.,0.));
#11372=DIRECTION('ref_axis',(1.,0.,0.));
#11373=DIRECTION('',(0.,-1.,0.));
#11374=DIRECTION('center_axis',(0.,-1.,0.));
#11375=DIRECTION('ref_axis',(1.,0.,0.));
#11376=DIRECTION('center_axis',(0.,1.,0.));
#11377=DIRECTION('ref_axis',(1.,0.,0.));
#11378=DIRECTION('center_axis',(0.,1.,0.));
#11379=DIRECTION('ref_axis',(1.,0.,0.));
#11380=DIRECTION('',(0.,-1.,0.));
#11381=DIRECTION('center_axis',(0.,1.,0.));
#11382=DIRECTION('ref_axis',(1.,0.,0.));
#11383=DIRECTION('center_axis',(0.,1.,0.));
#11384=DIRECTION('ref_axis',(1.,0.,0.));
#11385=DIRECTION('center_axis',(0.,1.,0.));
#11386=DIRECTION('ref_axis',(1.,0.,0.));
#11387=DIRECTION('axis',(0.,0.,1.));
#11388=DIRECTION('refdir',(1.,0.,0.));
#11389=DIRECTION('center_axis',(0.,1.,0.));
#11390=DIRECTION('ref_axis',(1.,0.,0.));
#11391=DIRECTION('center_axis',(0.,-1.,0.));
#11392=DIRECTION('ref_axis',(1.,0.,0.));
#11393=DIRECTION('',(0.,-1.,0.));
#11394=DIRECTION('center_axis',(0.,-1.,0.));
#11395=DIRECTION('ref_axis',(1.,0.,0.));
#11396=DIRECTION('center_axis',(0.,1.,0.));
#11397=DIRECTION('ref_axis',(1.,0.,0.));
#11398=DIRECTION('center_axis',(0.,1.,0.));
#11399=DIRECTION('ref_axis',(1.,0.,0.));
#11400=DIRECTION('',(0.,-1.,0.));
#11401=DIRECTION('center_axis',(0.,1.,0.));
#11402=DIRECTION('ref_axis',(1.,0.,0.));
#11403=DIRECTION('center_axis',(0.,1.,0.));
#11404=DIRECTION('ref_axis',(1.,0.,0.));
#11405=DIRECTION('center_axis',(0.,1.,0.));
#11406=DIRECTION('ref_axis',(1.,0.,0.));
#11407=DIRECTION('axis',(0.,0.,1.));
#11408=DIRECTION('refdir',(1.,0.,0.));
#11409=DIRECTION('center_axis',(0.,1.,0.));
#11410=DIRECTION('ref_axis',(1.,0.,0.));
#11411=DIRECTION('center_axis',(0.,-1.,0.));
#11412=DIRECTION('ref_axis',(1.,0.,0.));
#11413=DIRECTION('',(0.,-1.,0.));
#11414=DIRECTION('center_axis',(0.,-1.,0.));
#11415=DIRECTION('ref_axis',(1.,0.,0.));
#11416=DIRECTION('center_axis',(0.,1.,0.));
#11417=DIRECTION('ref_axis',(1.,0.,0.));
#11418=DIRECTION('center_axis',(0.,1.,0.));
#11419=DIRECTION('ref_axis',(1.,0.,0.));
#11420=DIRECTION('',(0.,-1.,0.));
#11421=DIRECTION('center_axis',(0.,1.,0.));
#11422=DIRECTION('ref_axis',(1.,0.,0.));
#11423=DIRECTION('center_axis',(0.,1.,0.));
#11424=DIRECTION('ref_axis',(1.,0.,0.));
#11425=DIRECTION('center_axis',(0.,1.,0.));
#11426=DIRECTION('ref_axis',(1.,0.,0.));
#11427=DIRECTION('axis',(0.,0.,1.));
#11428=DIRECTION('refdir',(1.,0.,0.));
#11429=DIRECTION('center_axis',(0.,0.,1.));
#11430=DIRECTION('ref_axis',(1.,0.,0.));
#11431=DIRECTION('',(0.,1.,0.));
#11432=DIRECTION('center_axis',(0.,0.,1.));
#11433=DIRECTION('ref_axis',(1.,0.,0.));
#11434=DIRECTION('center_axis',(0.,0.,1.));
#11435=DIRECTION('ref_axis',(1.,0.,0.));
#11436=DIRECTION('center_axis',(0.,0.,1.));
#11437=DIRECTION('ref_axis',(1.,0.,0.));
#11438=DIRECTION('',(0.,0.,1.));
#11439=DIRECTION('center_axis',(0.,0.,1.));
#11440=DIRECTION('ref_axis',(1.,0.,0.));
#11441=DIRECTION('center_axis',(0.,0.,1.));
#11442=DIRECTION('ref_axis',(1.,0.,0.));
#11443=DIRECTION('',(0.,-1.,0.));
#11444=DIRECTION('center_axis',(0.,1.,0.));
#11445=DIRECTION('ref_axis',(1.,0.,0.));
#11446=DIRECTION('center_axis',(0.,-1.,0.));
#11447=DIRECTION('ref_axis',(1.,0.,0.));
#11448=DIRECTION('',(0.,-1.,0.));
#11449=DIRECTION('center_axis',(0.,-1.,0.));
#11450=DIRECTION('ref_axis',(1.,0.,0.));
#11451=DIRECTION('center_axis',(0.,1.,0.));
#11452=DIRECTION('ref_axis',(1.,0.,0.));
#11453=DIRECTION('center_axis',(0.,1.,0.));
#11454=DIRECTION('ref_axis',(1.,0.,0.));
#11455=DIRECTION('',(0.,-1.,0.));
#11456=DIRECTION('center_axis',(0.,1.,0.));
#11457=DIRECTION('ref_axis',(1.,0.,0.));
#11458=DIRECTION('center_axis',(0.,1.,0.));
#11459=DIRECTION('ref_axis',(1.,0.,0.));
#11460=DIRECTION('center_axis',(0.,1.,0.));
#11461=DIRECTION('ref_axis',(1.,0.,0.));
#11462=DIRECTION('axis',(0.,0.,1.));
#11463=DIRECTION('refdir',(1.,0.,0.));
#11464=DIRECTION('center_axis',(0.,0.,1.));
#11465=DIRECTION('ref_axis',(1.,0.,0.));
#11466=DIRECTION('',(0.,1.,0.));
#11467=DIRECTION('center_axis',(0.,0.,1.));
#11468=DIRECTION('ref_axis',(1.,0.,0.));
#11469=DIRECTION('center_axis',(0.,0.,1.));
#11470=DIRECTION('ref_axis',(1.,0.,0.));
#11471=DIRECTION('center_axis',(0.,0.,1.));
#11472=DIRECTION('ref_axis',(1.,0.,0.));
#11473=DIRECTION('',(0.,0.,1.));
#11474=DIRECTION('center_axis',(0.,0.,1.));
#11475=DIRECTION('ref_axis',(1.,0.,0.));
#11476=DIRECTION('center_axis',(0.,0.,1.));
#11477=DIRECTION('ref_axis',(1.,0.,0.));
#11478=DIRECTION('',(0.,-1.,0.));
#11479=DIRECTION('center_axis',(0.,1.,0.));
#11480=DIRECTION('ref_axis',(1.,0.,0.));
#11481=DIRECTION('center_axis',(0.,-1.,0.));
#11482=DIRECTION('ref_axis',(1.,0.,0.));
#11483=DIRECTION('',(0.,-1.,0.));
#11484=DIRECTION('center_axis',(0.,-1.,0.));
#11485=DIRECTION('ref_axis',(1.,0.,0.));
#11486=DIRECTION('center_axis',(0.,1.,0.));
#11487=DIRECTION('ref_axis',(1.,0.,0.));
#11488=DIRECTION('center_axis',(0.,1.,0.));
#11489=DIRECTION('ref_axis',(1.,0.,0.));
#11490=DIRECTION('',(0.,-1.,0.));
#11491=DIRECTION('center_axis',(0.,1.,0.));
#11492=DIRECTION('ref_axis',(1.,0.,0.));
#11493=DIRECTION('center_axis',(0.,1.,0.));
#11494=DIRECTION('ref_axis',(1.,0.,0.));
#11495=DIRECTION('center_axis',(0.,1.,0.));
#11496=DIRECTION('ref_axis',(1.,0.,0.));
#11497=DIRECTION('axis',(0.,0.,1.));
#11498=DIRECTION('refdir',(1.,0.,0.));
#11499=DIRECTION('center_axis',(0.,0.,1.));
#11500=DIRECTION('ref_axis',(1.,0.,0.));
#11501=DIRECTION('',(0.,1.,0.));
#11502=DIRECTION('center_axis',(0.,0.,1.));
#11503=DIRECTION('ref_axis',(1.,0.,0.));
#11504=DIRECTION('center_axis',(0.,0.,1.));
#11505=DIRECTION('ref_axis',(1.,0.,0.));
#11506=DIRECTION('center_axis',(0.,0.,1.));
#11507=DIRECTION('ref_axis',(1.,0.,0.));
#11508=DIRECTION('',(0.,0.,1.));
#11509=DIRECTION('center_axis',(0.,0.,1.));
#11510=DIRECTION('ref_axis',(1.,0.,0.));
#11511=DIRECTION('center_axis',(0.,0.,1.));
#11512=DIRECTION('ref_axis',(1.,0.,0.));
#11513=DIRECTION('',(0.,-1.,0.));
#11514=DIRECTION('center_axis',(0.,1.,0.));
#11515=DIRECTION('ref_axis',(1.,0.,0.));
#11516=DIRECTION('center_axis',(0.,1.,0.));
#11517=DIRECTION('ref_axis',(1.,0.,0.));
#11518=DIRECTION('',(0.,1.,0.));
#11519=DIRECTION('center_axis',(0.,-1.,0.));
#11520=DIRECTION('ref_axis',(1.,0.,0.));
#11521=DIRECTION('center_axis',(0.,1.,0.));
#11522=DIRECTION('ref_axis',(1.,0.,0.));
#11523=DIRECTION('center_axis',(0.,1.,0.));
#11524=DIRECTION('ref_axis',(1.,0.,0.));
#11525=DIRECTION('',(0.,1.,0.));
#11526=DIRECTION('center_axis',(0.,-1.,0.));
#11527=DIRECTION('ref_axis',(1.,0.,0.));
#11528=DIRECTION('center_axis',(0.,1.,0.));
#11529=DIRECTION('ref_axis',(1.,0.,0.));
#11530=DIRECTION('center_axis',(0.,1.,0.));
#11531=DIRECTION('ref_axis',(1.,0.,0.));
#11532=DIRECTION('',(0.,1.,0.));
#11533=DIRECTION('center_axis',(0.,-1.,0.));
#11534=DIRECTION('ref_axis',(1.,0.,0.));
#11535=DIRECTION('center_axis',(0.,1.,0.));
#11536=DIRECTION('ref_axis',(1.,0.,0.));
#11537=DIRECTION('center_axis',(0.,1.,0.));
#11538=DIRECTION('ref_axis',(1.,0.,0.));
#11539=DIRECTION('',(0.,1.,0.));
#11540=DIRECTION('center_axis',(0.,-1.,0.));
#11541=DIRECTION('ref_axis',(1.,0.,0.));
#11542=DIRECTION('center_axis',(0.,1.,0.));
#11543=DIRECTION('ref_axis',(1.,0.,0.));
#11544=DIRECTION('center_axis',(0.,1.,0.));
#11545=DIRECTION('ref_axis',(1.,0.,0.));
#11546=DIRECTION('center_axis',(0.,1.,0.));
#11547=DIRECTION('ref_axis',(1.,0.,0.));
#11548=DIRECTION('center_axis',(0.,1.,0.));
#11549=DIRECTION('ref_axis',(1.,0.,0.));
#11550=DIRECTION('',(0.,-1.,0.));
#11551=DIRECTION('center_axis',(0.,1.,0.));
#11552=DIRECTION('ref_axis',(1.,0.,0.));
#11553=DIRECTION('center_axis',(0.,1.,0.));
#11554=DIRECTION('ref_axis',(1.,0.,0.));
#11555=DIRECTION('center_axis',(0.,-1.,0.));
#11556=DIRECTION('ref_axis',(1.,0.,0.));
#11557=DIRECTION('',(0.,-1.,0.));
#11558=DIRECTION('center_axis',(0.,-1.,0.));
#11559=DIRECTION('ref_axis',(1.,0.,0.));
#11560=DIRECTION('center_axis',(0.,1.,0.));
#11561=DIRECTION('ref_axis',(1.,0.,0.));
#11562=DIRECTION('center_axis',(0.,1.,0.));
#11563=DIRECTION('ref_axis',(1.,0.,0.));
#11564=DIRECTION('',(0.,-1.,0.));
#11565=DIRECTION('center_axis',(0.,1.,0.));
#11566=DIRECTION('ref_axis',(1.,0.,0.));
#11567=DIRECTION('center_axis',(0.,1.,0.));
#11568=DIRECTION('ref_axis',(1.,0.,0.));
#11569=DIRECTION('axis',(0.,0.,1.));
#11570=DIRECTION('refdir',(1.,0.,0.));
#11571=DIRECTION('center_axis',(0.866025403784439,0.,-0.5));
#11572=DIRECTION('ref_axis',(0.5,0.,0.866025403784439));
#11573=DIRECTION('',(0.5,0.,0.866025403784439));
#11574=DIRECTION('',(0.,-1.,0.));
#11575=DIRECTION('',(0.5,0.,0.866025403784439));
#11576=DIRECTION('',(0.,-1.,0.));
#11577=DIRECTION('center_axis',(1.92296268638356E-16,0.,-1.));
#11578=DIRECTION('ref_axis',(1.,0.,1.92296268638356E-16));
#11579=DIRECTION('',(1.,0.,1.92296268638356E-16));
#11580=DIRECTION('',(0.,-1.,0.));
#11581=DIRECTION('',(1.,0.,1.92296268638356E-16));
#11582=DIRECTION('center_axis',(-0.866025403784439,0.,-0.5));
#11583=DIRECTION('ref_axis',(0.5,0.,-0.866025403784439));
#11584=DIRECTION('',(0.5,0.,-0.866025403784439));
#11585=DIRECTION('',(0.,-1.,0.));
#11586=DIRECTION('',(0.5,0.,-0.866025403784438));
#11587=DIRECTION('center_axis',(-0.866025403784439,0.,0.5));
#11588=DIRECTION('ref_axis',(-0.5,0.,-0.866025403784439));
#11589=DIRECTION('',(-0.5,0.,-0.866025403784439));
#11590=DIRECTION('',(0.,-1.,0.));
#11591=DIRECTION('',(-0.5,0.,-0.866025403784439));
#11592=DIRECTION('center_axis',(-1.92296268638356E-16,0.,1.));
#11593=DIRECTION('ref_axis',(-1.,0.,-1.92296268638356E-16));
#11594=DIRECTION('',(-1.,0.,-1.92296268638356E-16));
#11595=DIRECTION('',(0.,-1.,0.));
#11596=DIRECTION('',(-1.,0.,-1.92296268638356E-16));
#11597=DIRECTION('center_axis',(0.866025403784439,0.,0.5));
#11598=DIRECTION('ref_axis',(-0.5,0.,0.866025403784439));
#11599=DIRECTION('',(-0.5,0.,0.866025403784439));
#11600=DIRECTION('',(-0.5,0.,0.866025403784439));
#11601=DIRECTION('center_axis',(0.,-1.,0.));
#11602=DIRECTION('ref_axis',(0.,0.,-1.));
#11603=DIRECTION('center_axis',(0.,1.,0.));
#11604=DIRECTION('ref_axis',(0.,0.,1.));
#11605=DIRECTION('center_axis',(0.,-1.,0.));
#11606=DIRECTION('ref_axis',(1.,0.,0.));
#11607=DIRECTION('center_axis',(0.,-1.,0.));
#11608=DIRECTION('ref_axis',(1.,0.,0.));
#11609=DIRECTION('center_axis',(0.,-1.,0.));
#11610=DIRECTION('ref_axis',(1.,0.,0.));
#11611=DIRECTION('',(0.707106781186547,0.707106781186548,8.65956056235493E-17));
#11612=DIRECTION('center_axis',(0.,-1.,0.));
#11613=DIRECTION('ref_axis',(1.,0.,0.));
#11614=DIRECTION('center_axis',(0.,1.,0.));
#11615=DIRECTION('ref_axis',(1.,0.,0.));
#11616=DIRECTION('',(0.,1.,0.));
#11617=DIRECTION('center_axis',(0.,1.,0.));
#11618=DIRECTION('ref_axis',(1.,0.,0.));
#11619=DIRECTION('center_axis',(0.,-1.,0.));
#11620=DIRECTION('ref_axis',(1.,0.,0.));
#11621=DIRECTION('',(-0.707106781186547,0.707106781186548,-8.65956056235493E-17));
#11622=DIRECTION('center_axis',(0.,-1.,0.));
#11623=DIRECTION('ref_axis',(0.,0.,-1.));
#11624=DIRECTION('',(0.,0.,1.));
#11625=DIRECTION('',(1.,0.,0.));
#11626=DIRECTION('',(0.,0.,1.));
#11627=DIRECTION('',(1.,0.,0.));
#11628=DIRECTION('',(0.,0.,1.));
#11629=DIRECTION('',(1.,0.,0.));
#11630=DIRECTION('',(0.,0.,1.));
#11631=DIRECTION('',(1.,0.,0.));
#11632=DIRECTION('',(0.,0.,1.));
#11633=DIRECTION('',(1.,0.,0.));
#11634=DIRECTION('',(0.,0.,1.));
#11635=DIRECTION('',(1.,0.,0.));
#11636=DIRECTION('',(0.,0.,1.));
#11637=DIRECTION('',(1.,0.,0.));
#11638=DIRECTION('',(0.,0.,1.));
#11639=DIRECTION('',(1.,0.,0.));
#11640=DIRECTION('',(0.,0.,1.));
#11641=DIRECTION('',(1.,0.,0.));
#11642=DIRECTION('',(0.,0.,1.));
#11643=DIRECTION('',(1.,0.,0.));
#11644=DIRECTION('',(0.,-1.,2.22044604925031E-16));
#11645=DIRECTION('',(1.,0.,0.));
#11646=DIRECTION('',(0.,-1.,2.22044604925031E-16));
#11647=DIRECTION('',(1.,0.,0.));
#11648=DIRECTION('',(0.,-1.,2.22044604925031E-16));
#11649=DIRECTION('',(1.,0.,0.));
#11650=DIRECTION('',(0.,-1.,2.22044604925031E-16));
#11651=DIRECTION('',(1.,0.,0.));
#11652=DIRECTION('',(0.,-1.,2.22044604925031E-16));
#11653=DIRECTION('',(1.,0.,0.));
#11654=DIRECTION('',(0.,0.,1.));
#11655=DIRECTION('',(1.,0.,0.));
#11656=DIRECTION('',(0.,0.,1.));
#11657=DIRECTION('',(1.,0.,0.));
#11658=CARTESIAN_POINT('',(0.,0.,0.));
#11659=CARTESIAN_POINT('',(0.,0.,0.));
#11660=CARTESIAN_POINT('',(0.,0.,0.));
#11661=CARTESIAN_POINT('Origin',(4.4,3.4,-0.1));
#11662=CARTESIAN_POINT('',(4.235,3.4,0.));
#11663=CARTESIAN_POINT('Origin',(4.4,3.4,0.));
#11664=CARTESIAN_POINT('',(4.235,3.4,1.));
#11665=CARTESIAN_POINT('',(4.235,3.4,-0.1));
#11666=CARTESIAN_POINT('Origin',(4.4,3.4,1.));
#11667=CARTESIAN_POINT('Origin',(4.4,-3.4,-0.1));
#11668=CARTESIAN_POINT('',(4.235,-3.4,0.));
#11669=CARTESIAN_POINT('Origin',(4.4,-3.4,0.));
#11670=CARTESIAN_POINT('',(4.235,-3.4,1.));
#11671=CARTESIAN_POINT('',(4.235,-3.4,-0.1));
#11672=CARTESIAN_POINT('Origin',(4.4,-3.4,1.));
#11673=CARTESIAN_POINT('Origin',(-4.4,3.4,-0.1));
#11674=CARTESIAN_POINT('',(-4.565,3.4,0.));
#11675=CARTESIAN_POINT('Origin',(-4.4,3.4,0.));
#11676=CARTESIAN_POINT('',(-4.565,3.4,1.));
#11677=CARTESIAN_POINT('',(-4.565,3.4,-0.1));
#11678=CARTESIAN_POINT('Origin',(-4.4,3.4,1.));
#11679=CARTESIAN_POINT('Origin',(-4.4,-3.4,-0.1));
#11680=CARTESIAN_POINT('',(-4.565,-3.4,0.));
#11681=CARTESIAN_POINT('Origin',(-4.4,-3.4,0.));
#11682=CARTESIAN_POINT('',(-4.565,-3.4,1.));
#11683=CARTESIAN_POINT('',(-4.565,-3.4,-0.1));
#11684=CARTESIAN_POINT('Origin',(-4.4,-3.4,1.));
#11685=CARTESIAN_POINT('Origin',(11.4,-1.4,-0.1));
#11686=CARTESIAN_POINT('',(11.19,-1.4,0.));
#11687=CARTESIAN_POINT('Origin',(11.4,-1.4,0.));
#11688=CARTESIAN_POINT('',(11.19,-1.4,1.));
#11689=CARTESIAN_POINT('',(11.19,-1.4,-0.1));
#11690=CARTESIAN_POINT('Origin',(11.4,-1.4,1.));
#11691=CARTESIAN_POINT('Origin',(8.6,1.4,-0.1));
#11692=CARTESIAN_POINT('',(8.39,1.4,0.));
#11693=CARTESIAN_POINT('Origin',(8.6,1.4,0.));
#11694=CARTESIAN_POINT('',(8.39,1.4,1.));
#11695=CARTESIAN_POINT('',(8.39,1.4,-0.1));
#11696=CARTESIAN_POINT('Origin',(8.6,1.4,1.));
#11697=CARTESIAN_POINT('Origin',(8.6,-1.4,-0.1));
#11698=CARTESIAN_POINT('',(8.39,-1.4,0.));
#11699=CARTESIAN_POINT('Origin',(8.6,-1.4,0.));
#11700=CARTESIAN_POINT('',(8.39,-1.4,1.));
#11701=CARTESIAN_POINT('',(8.39,-1.4,-0.1));
#11702=CARTESIAN_POINT('Origin',(8.6,-1.4,1.));
#11703=CARTESIAN_POINT('Origin',(11.4,1.4,-0.1));
#11704=CARTESIAN_POINT('',(11.19,1.4,0.));
#11705=CARTESIAN_POINT('Origin',(11.4,1.4,0.));
#11706=CARTESIAN_POINT('',(11.19,1.4,1.));
#11707=CARTESIAN_POINT('',(11.19,1.4,-0.1));
#11708=CARTESIAN_POINT('Origin',(11.4,1.4,1.));
#11709=CARTESIAN_POINT('Origin',(-2.7,7.,-0.1));
#11710=CARTESIAN_POINT('',(-2.95,7.,0.));
#11711=CARTESIAN_POINT('Origin',(-2.7,7.,0.));
#11712=CARTESIAN_POINT('',(-2.95,7.,1.));
#11713=CARTESIAN_POINT('',(-2.95,7.,-0.1));
#11714=CARTESIAN_POINT('Origin',(-2.7,7.,1.));
#11715=CARTESIAN_POINT('Origin',(2.7,7.,-0.1));
#11716=CARTESIAN_POINT('',(2.45,7.,0.));
#11717=CARTESIAN_POINT('Origin',(2.7,7.,0.));
#11718=CARTESIAN_POINT('',(2.45,7.,1.));
#11719=CARTESIAN_POINT('',(2.45,7.,-0.1));
#11720=CARTESIAN_POINT('Origin',(2.7,7.,1.));
#11721=CARTESIAN_POINT('Origin',(-2.7,-7.,-0.1));
#11722=CARTESIAN_POINT('',(-2.95,-7.,0.));
#11723=CARTESIAN_POINT('Origin',(-2.7,-7.,0.));
#11724=CARTESIAN_POINT('',(-2.95,-7.,1.));
#11725=CARTESIAN_POINT('',(-2.95,-7.,-0.1));
#11726=CARTESIAN_POINT('Origin',(-2.7,-7.,1.));
#11727=CARTESIAN_POINT('Origin',(2.7,-7.,-0.1));
#11728=CARTESIAN_POINT('',(2.45,-7.,0.));
#11729=CARTESIAN_POINT('Origin',(2.7,-7.,0.));
#11730=CARTESIAN_POINT('',(2.45,-7.,1.));
#11731=CARTESIAN_POINT('',(2.45,-7.,-0.1));
#11732=CARTESIAN_POINT('Origin',(2.7,-7.,1.));
#11733=CARTESIAN_POINT('Origin',(12.5,11.,0.));
#11734=CARTESIAN_POINT('',(12.5,11.,0.));
#11735=CARTESIAN_POINT('',(-6.5,11.,0.));
#11736=CARTESIAN_POINT('',(12.5,11.,0.));
#11737=CARTESIAN_POINT('',(-6.5,11.,1.));
#11738=CARTESIAN_POINT('',(-6.5,11.,0.));
#11739=CARTESIAN_POINT('',(12.5,11.,1.));
#11740=CARTESIAN_POINT('',(12.5,11.,1.));
#11741=CARTESIAN_POINT('',(12.5,11.,0.));
#11742=CARTESIAN_POINT('Origin',(12.5,-11.,0.));
#11743=CARTESIAN_POINT('',(12.5,-11.,0.));
#11744=CARTESIAN_POINT('',(12.5,-11.,0.));
#11745=CARTESIAN_POINT('',(12.5,-11.,1.));
#11746=CARTESIAN_POINT('',(12.5,-11.,1.));
#11747=CARTESIAN_POINT('',(12.5,-11.,0.));
#11748=CARTESIAN_POINT('Origin',(-6.5,-11.,0.));
#11749=CARTESIAN_POINT('',(-6.5,-11.,0.));
#11750=CARTESIAN_POINT('',(-6.5,-11.,0.));
#11751=CARTESIAN_POINT('',(-6.5,-11.,1.));
#11752=CARTESIAN_POINT('',(-6.5,-11.,1.));
#11753=CARTESIAN_POINT('',(-6.5,-11.,0.));
#11754=CARTESIAN_POINT('Origin',(-6.5,11.,0.));
#11755=CARTESIAN_POINT('',(-6.5,11.,0.));
#11756=CARTESIAN_POINT('',(-6.5,11.,1.));
#11757=CARTESIAN_POINT('Origin',(3.,0.,1.));
#11758=CARTESIAN_POINT('Origin',(3.,0.,0.));
#11759=CARTESIAN_POINT('',(0.,0.,0.));
#11760=CARTESIAN_POINT('Origin',(-2.,-7.9,7.));
#11761=CARTESIAN_POINT('',(-2.165,-7.8,7.));
#11762=CARTESIAN_POINT('Origin',(-2.,-7.8,7.));
#11763=CARTESIAN_POINT('',(-2.165,-6.2,7.));
#11764=CARTESIAN_POINT('',(-2.165,-7.9,7.));
#11765=CARTESIAN_POINT('Origin',(-2.,-6.2,7.));
#11766=CARTESIAN_POINT('Origin',(1.22464679914735E-16,-7.9,9.));
#11767=CARTESIAN_POINT('',(-0.165,-7.8,9.));
#11768=CARTESIAN_POINT('Origin',(1.22464679914735E-16,-7.8,9.));
#11769=CARTESIAN_POINT('',(-0.165,-6.2,9.));
#11770=CARTESIAN_POINT('',(-0.165,-7.9,9.));
#11771=CARTESIAN_POINT('Origin',(1.22464679914735E-16,-6.2,9.));
#11772=CARTESIAN_POINT('Origin',(2.,-7.9,7.));
#11773=CARTESIAN_POINT('',(1.835,-7.8,7.));
#11774=CARTESIAN_POINT('Origin',(2.,-7.8,7.));
#11775=CARTESIAN_POINT('',(1.835,-6.2,7.));
#11776=CARTESIAN_POINT('',(1.835,-7.9,7.));
#11777=CARTESIAN_POINT('Origin',(2.,-6.2,7.));
#11778=CARTESIAN_POINT('Origin',(-3.67394039744206E-16,-7.9,5.));
#11779=CARTESIAN_POINT('',(-0.165,-7.8,5.));
#11780=CARTESIAN_POINT('Origin',(-3.67394039744206E-16,-7.8,5.));
#11781=CARTESIAN_POINT('',(-0.165,-6.2,5.));
#11782=CARTESIAN_POINT('',(-0.165,-7.9,5.));
#11783=CARTESIAN_POINT('Origin',(-3.67394039744206E-16,-6.2,5.));
#11784=CARTESIAN_POINT('Origin',(-2.7,-7.,4.3));
#11785=CARTESIAN_POINT('',(-2.20625,-6.65910274641763,4.3));
#11786=CARTESIAN_POINT('',(-2.20625,-7.34089725358237,4.3));
#11787=CARTESIAN_POINT('',(-2.20625,-7.4,4.3));
#11788=CARTESIAN_POINT('Origin',(-2.7,-7.,4.3));
#11789=CARTESIAN_POINT('Origin',(-2.7,-7.,1.8));
#11790=CARTESIAN_POINT('',(-3.3,-7.,1.8));
#11791=CARTESIAN_POINT('Origin',(-2.7,-7.,1.8));
#11792=CARTESIAN_POINT('',(-3.3,-7.,2.35555555555556));
#11793=CARTESIAN_POINT('',(-3.3,-7.,1.8));
#11794=CARTESIAN_POINT('Origin',(-2.7,-7.,3.42222222222222));
#11795=CARTESIAN_POINT('Origin',(-2.7,-7.,3.42222222222222));
#11796=CARTESIAN_POINT('Origin',(-2.7,-7.,1.8));
#11797=CARTESIAN_POINT('',(-3.03,-7.,1.8));
#11798=CARTESIAN_POINT('Origin',(-2.7,-7.,1.8));
#11799=CARTESIAN_POINT('Origin',(2.7,-7.,4.3));
#11800=CARTESIAN_POINT('',(2.20625,-7.34089725358236,4.3));
#11801=CARTESIAN_POINT('',(2.20625,-6.65910274641764,4.3));
#11802=CARTESIAN_POINT('',(2.20625,-7.4,4.3));
#11803=CARTESIAN_POINT('',(2.1,-7.,4.3));
#11804=CARTESIAN_POINT('Origin',(2.7,-7.,4.3));
#11805=CARTESIAN_POINT('Origin',(2.7,-7.,4.3));
#11806=CARTESIAN_POINT('Origin',(2.7,-7.,1.8));
#11807=CARTESIAN_POINT('',(2.1,-7.,1.8));
#11808=CARTESIAN_POINT('Origin',(2.7,-7.,1.8));
#11809=CARTESIAN_POINT('',(2.1,-7.,1.8));
#11810=CARTESIAN_POINT('Origin',(2.7,-7.,3.42222222222222));
#11811=CARTESIAN_POINT('Origin',(2.7,-7.,1.8));
#11812=CARTESIAN_POINT('',(2.37,-7.,1.8));
#11813=CARTESIAN_POINT('Origin',(2.7,-7.,1.8));
#11814=CARTESIAN_POINT('Origin',(-2.7,-7.,0.9));
#11815=CARTESIAN_POINT('',(-3.03,-7.,1.));
#11816=CARTESIAN_POINT('Origin',(-2.7,-7.,1.));
#11817=CARTESIAN_POINT('',(-3.03,-7.,0.9));
#11818=CARTESIAN_POINT('Origin',(2.7,-7.,0.9));
#11819=CARTESIAN_POINT('',(2.37,-7.,1.));
#11820=CARTESIAN_POINT('Origin',(2.7,-7.,1.));
#11821=CARTESIAN_POINT('',(2.37,-7.,0.9));
#11822=CARTESIAN_POINT('Origin',(1.7,-7.8,5.2));
#11823=CARTESIAN_POINT('',(1.71218189678592,-7.8,5.17834329460281));
#11824=CARTESIAN_POINT('',(1.71218189678592,-6.2,5.17834329460281));
#11825=CARTESIAN_POINT('',(1.71218189678592,-7.8,5.17834329460281));
#11826=CARTESIAN_POINT('',(3.5,-7.8,2.));
#11827=CARTESIAN_POINT('',(3.5,-7.8,2.));
#11828=CARTESIAN_POINT('',(3.5,-6.2,2.));
#11829=CARTESIAN_POINT('',(3.5,-7.8,2.));
#11830=CARTESIAN_POINT('',(3.5,-6.2,2.));
#11831=CARTESIAN_POINT('Origin',(-3.5,-7.8,2.));
#11832=CARTESIAN_POINT('',(-1.71218189678592,-6.2,5.17834329460281));
#11833=CARTESIAN_POINT('',(-1.71218189678592,-7.8,5.17834329460281));
#11834=CARTESIAN_POINT('',(-1.71218189678592,-7.8,5.17834329460281));
#11835=CARTESIAN_POINT('',(-3.5,-6.2,2.));
#11836=CARTESIAN_POINT('',(-1.7,-6.2,5.2));
#11837=CARTESIAN_POINT('',(-3.5,-7.8,2.));
#11838=CARTESIAN_POINT('',(-3.5,-7.8,2.));
#11839=CARTESIAN_POINT('',(-1.7,-7.8,5.2));
#11840=CARTESIAN_POINT('Origin',(-3.5,-7.8,1.));
#11841=CARTESIAN_POINT('',(-3.5,-7.8,1.));
#11842=CARTESIAN_POINT('',(-3.5,-7.8,2.));
#11843=CARTESIAN_POINT('',(-3.5,-6.2,1.));
#11844=CARTESIAN_POINT('',(-3.5,-6.2,2.));
#11845=CARTESIAN_POINT('',(-3.5,-7.8,1.));
#11846=CARTESIAN_POINT('Origin',(3.5,-7.8,1.));
#11847=CARTESIAN_POINT('',(3.5,-7.8,1.));
#11848=CARTESIAN_POINT('',(-3.5,-7.8,1.));
#11849=CARTESIAN_POINT('',(3.5,-6.2,1.));
#11850=CARTESIAN_POINT('',(-3.5,-6.2,1.));
#11851=CARTESIAN_POINT('',(3.5,-7.8,1.));
#11852=CARTESIAN_POINT('Origin',(3.5,-7.8,2.));
#11853=CARTESIAN_POINT('',(3.5,-7.8,1.));
#11854=CARTESIAN_POINT('',(3.5,-6.2,1.));
#11855=CARTESIAN_POINT('Origin',(0.,-6.2,7.));
#11856=CARTESIAN_POINT('Origin',(0.,-6.2,7.));
#11857=CARTESIAN_POINT('',(-1.6,-6.2,7.));
#11858=CARTESIAN_POINT('Origin',(0.,-6.2,7.));
#11859=CARTESIAN_POINT('Origin',(0.,-7.8,7.));
#11860=CARTESIAN_POINT('',(-1.6,-7.8,7.));
#11861=CARTESIAN_POINT('',(-1.6,-7.8,7.));
#11862=CARTESIAN_POINT('Origin',(0.,-7.8,7.));
#11863=CARTESIAN_POINT('Origin',(0.,-7.8,7.));
#11864=CARTESIAN_POINT('Origin',(0.,-7.8,7.));
#11865=CARTESIAN_POINT('Origin',(0.,-7.8,7.));
#11866=CARTESIAN_POINT('',(0.,0.,0.));
#11867=CARTESIAN_POINT('Origin',(-2.,-8.2,7.));
#11868=CARTESIAN_POINT('',(-2.225,-8.1,7.));
#11869=CARTESIAN_POINT('Origin',(-2.,-8.1,7.));
#11870=CARTESIAN_POINT('',(-2.225,-7.8,7.));
#11871=CARTESIAN_POINT('',(-2.225,-8.2,7.));
#11872=CARTESIAN_POINT('Origin',(-2.,-7.8,7.));
#11873=CARTESIAN_POINT('Origin',(1.22464679914735E-16,-8.2,9.));
#11874=CARTESIAN_POINT('',(-0.225,-8.1,9.));
#11875=CARTESIAN_POINT('Origin',(1.22464679914735E-16,-8.1,9.));
#11876=CARTESIAN_POINT('',(-0.225,-7.8,9.));
#11877=CARTESIAN_POINT('',(-0.225,-8.2,9.));
#11878=CARTESIAN_POINT('Origin',(1.22464679914735E-16,-7.8,9.));
#11879=CARTESIAN_POINT('Origin',(2.,-8.2,7.));
#11880=CARTESIAN_POINT('',(1.775,-8.1,7.));
#11881=CARTESIAN_POINT('Origin',(2.,-8.1,7.));
#11882=CARTESIAN_POINT('',(1.775,-7.8,7.));
#11883=CARTESIAN_POINT('',(1.775,-8.2,7.));
#11884=CARTESIAN_POINT('Origin',(2.,-7.8,7.));
#11885=CARTESIAN_POINT('Origin',(-3.67394039744206E-16,-8.2,5.));
#11886=CARTESIAN_POINT('',(-0.225,-8.1,5.));
#11887=CARTESIAN_POINT('Origin',(-3.67394039744206E-16,-8.1,5.));
#11888=CARTESIAN_POINT('',(-0.225,-7.8,5.));
#11889=CARTESIAN_POINT('',(-0.225,-8.2,5.));
#11890=CARTESIAN_POINT('Origin',(-3.67394039744206E-16,-7.8,5.));
#11891=CARTESIAN_POINT('Origin',(0.,-7.8,7.));
#11892=CARTESIAN_POINT('',(-1.59,-7.5,7.));
#11893=CARTESIAN_POINT('Origin',(0.,-7.5,7.));
#11894=CARTESIAN_POINT('',(-1.59,-7.8,7.));
#11895=CARTESIAN_POINT('',(-1.59,-7.8,7.));
#11896=CARTESIAN_POINT('Origin',(0.,-7.8,7.));
#11897=CARTESIAN_POINT('Origin',(0.,-7.5,7.));
#11898=CARTESIAN_POINT('',(-1.1,-7.5,7.));
#11899=CARTESIAN_POINT('Origin',(0.,-7.5,7.));
#11900=CARTESIAN_POINT('Origin',(0.,-8.1,7.));
#11901=CARTESIAN_POINT('',(-1.1,-8.1,7.));
#11902=CARTESIAN_POINT('',(-1.1,-8.1,7.));
#11903=CARTESIAN_POINT('Origin',(0.,-8.1,7.));
#11904=CARTESIAN_POINT('Origin',(0.,-8.1,7.));
#11905=CARTESIAN_POINT('',(-2.5,-7.8,7.));
#11906=CARTESIAN_POINT('Origin',(0.,-7.8,7.));
#11907=CARTESIAN_POINT('',(-2.5,-8.1,7.));
#11908=CARTESIAN_POINT('',(-2.5,-8.1,7.));
#11909=CARTESIAN_POINT('Origin',(0.,-8.1,7.));
#11910=CARTESIAN_POINT('Origin',(0.,-7.8,7.));
#11911=CARTESIAN_POINT('Origin',(0.,-8.1,7.));
#11912=CARTESIAN_POINT('',(0.,0.,0.));
#11913=CARTESIAN_POINT('Origin',(-2.,-6.3,7.));
#11914=CARTESIAN_POINT('',(-2.225,-6.2,7.));
#11915=CARTESIAN_POINT('Origin',(-2.,-6.2,7.));
#11916=CARTESIAN_POINT('',(-2.225,-5.9,7.));
#11917=CARTESIAN_POINT('',(-2.225,-6.3,7.));
#11918=CARTESIAN_POINT('Origin',(-2.,-5.9,7.));
#11919=CARTESIAN_POINT('Origin',(1.22464679914735E-16,-6.3,9.));
#11920=CARTESIAN_POINT('',(-0.225,-6.2,9.));
#11921=CARTESIAN_POINT('Origin',(1.22464679914735E-16,-6.2,9.));
#11922=CARTESIAN_POINT('',(-0.225,-5.9,9.));
#11923=CARTESIAN_POINT('',(-0.225,-6.3,9.));
#11924=CARTESIAN_POINT('Origin',(1.22464679914735E-16,-5.9,9.));
#11925=CARTESIAN_POINT('Origin',(2.,-6.3,7.));
#11926=CARTESIAN_POINT('',(1.775,-6.2,7.));
#11927=CARTESIAN_POINT('Origin',(2.,-6.2,7.));
#11928=CARTESIAN_POINT('',(1.775,-5.9,7.));
#11929=CARTESIAN_POINT('',(1.775,-6.3,7.));
#11930=CARTESIAN_POINT('Origin',(2.,-5.9,7.));
#11931=CARTESIAN_POINT('Origin',(-3.67394039744206E-16,-6.3,5.));
#11932=CARTESIAN_POINT('',(-0.225,-6.2,5.));
#11933=CARTESIAN_POINT('Origin',(-3.67394039744206E-16,-6.2,5.));
#11934=CARTESIAN_POINT('',(-0.225,-5.9,5.));
#11935=CARTESIAN_POINT('',(-0.225,-6.3,5.));
#11936=CARTESIAN_POINT('Origin',(-3.67394039744206E-16,-5.9,5.));
#11937=CARTESIAN_POINT('Origin',(0.,-6.5,7.));
#11938=CARTESIAN_POINT('',(-1.59,-6.2,7.));
#11939=CARTESIAN_POINT('Origin',(0.,-6.2,7.));
#11940=CARTESIAN_POINT('',(-1.59,-6.5,7.));
#11941=CARTESIAN_POINT('',(-1.59,-6.5,7.));
#11942=CARTESIAN_POINT('Origin',(0.,-6.5,7.));
#11943=CARTESIAN_POINT('Origin',(0.,-6.5,7.));
#11944=CARTESIAN_POINT('',(-1.1,-6.5,7.));
#11945=CARTESIAN_POINT('Origin',(0.,-6.5,7.));
#11946=CARTESIAN_POINT('Origin',(0.,-6.2,7.));
#11947=CARTESIAN_POINT('',(-1.1,-5.9,7.));
#11948=CARTESIAN_POINT('Origin',(0.,-5.9,7.));
#11949=CARTESIAN_POINT('',(-1.1,-6.2,7.));
#11950=CARTESIAN_POINT('Origin',(0.,-6.2,7.));
#11951=CARTESIAN_POINT('',(-2.5,-5.9,7.));
#11952=CARTESIAN_POINT('Origin',(0.,-5.9,7.));
#11953=CARTESIAN_POINT('',(-2.5,-6.2,7.));
#11954=CARTESIAN_POINT('',(-2.5,-6.2,7.));
#11955=CARTESIAN_POINT('Origin',(0.,-6.2,7.));
#11956=CARTESIAN_POINT('Origin',(0.,-5.9,7.));
#11957=CARTESIAN_POINT('Origin',(0.,-6.2,7.));
#11958=CARTESIAN_POINT('',(0.,0.,0.));
#11959=CARTESIAN_POINT('Origin',(-2.,6.1,7.));
#11960=CARTESIAN_POINT('',(-2.165,6.2,7.));
#11961=CARTESIAN_POINT('Origin',(-2.,6.2,7.));
#11962=CARTESIAN_POINT('',(-2.165,7.8,7.));
#11963=CARTESIAN_POINT('',(-2.165,6.1,7.));
#11964=CARTESIAN_POINT('Origin',(-2.,7.8,7.));
#11965=CARTESIAN_POINT('Origin',(1.22464679914735E-16,6.1,9.));
#11966=CARTESIAN_POINT('',(-0.165,6.2,9.));
#11967=CARTESIAN_POINT('Origin',(1.22464679914735E-16,6.2,9.));
#11968=CARTESIAN_POINT('',(-0.165,7.8,9.));
#11969=CARTESIAN_POINT('',(-0.165,6.1,9.));
#11970=CARTESIAN_POINT('Origin',(1.22464679914735E-16,7.8,9.));
#11971=CARTESIAN_POINT('Origin',(2.,6.1,7.));
#11972=CARTESIAN_POINT('',(1.835,6.2,7.));
#11973=CARTESIAN_POINT('Origin',(2.,6.2,7.));
#11974=CARTESIAN_POINT('',(1.835,7.8,7.));
#11975=CARTESIAN_POINT('',(1.835,6.1,7.));
#11976=CARTESIAN_POINT('Origin',(2.,7.8,7.));
#11977=CARTESIAN_POINT('Origin',(-3.67394039744206E-16,6.1,5.));
#11978=CARTESIAN_POINT('',(-0.165,6.2,5.));
#11979=CARTESIAN_POINT('Origin',(-3.67394039744206E-16,6.2,5.));
#11980=CARTESIAN_POINT('',(-0.165,7.8,5.));
#11981=CARTESIAN_POINT('',(-0.165,6.1,5.));
#11982=CARTESIAN_POINT('Origin',(-3.67394039744206E-16,7.8,5.));
#11983=CARTESIAN_POINT('Origin',(-2.7,7.,4.3));
#11984=CARTESIAN_POINT('',(-2.20625,7.34089725358237,4.3));
#11985=CARTESIAN_POINT('',(-2.20625,6.65910274641763,4.3));
#11986=CARTESIAN_POINT('',(-2.20625,6.6,4.3));
#11987=CARTESIAN_POINT('Origin',(-2.7,7.,4.3));
#11988=CARTESIAN_POINT('Origin',(-2.7,7.,1.8));
#11989=CARTESIAN_POINT('',(-3.3,7.,1.8));
#11990=CARTESIAN_POINT('Origin',(-2.7,7.,1.8));
#11991=CARTESIAN_POINT('',(-3.3,7.,2.35555555555556));
#11992=CARTESIAN_POINT('',(-3.3,7.,1.8));
#11993=CARTESIAN_POINT('Origin',(-2.7,7.,3.42222222222222));
#11994=CARTESIAN_POINT('Origin',(-2.7,7.,3.42222222222222));
#11995=CARTESIAN_POINT('Origin',(-2.7,7.,1.8));
#11996=CARTESIAN_POINT('',(-3.03,7.,1.8));
#11997=CARTESIAN_POINT('Origin',(-2.7,7.,1.8));
#11998=CARTESIAN_POINT('Origin',(2.7,7.,4.3));
#11999=CARTESIAN_POINT('',(2.20625,6.65910274641764,4.3));
#12000=CARTESIAN_POINT('',(2.20625,7.34089725358236,4.3));
#12001=CARTESIAN_POINT('',(2.20625,6.6,4.3));
#12002=CARTESIAN_POINT('',(2.1,7.,4.3));
#12003=CARTESIAN_POINT('Origin',(2.7,7.,4.3));
#12004=CARTESIAN_POINT('Origin',(2.7,7.,4.3));
#12005=CARTESIAN_POINT('Origin',(2.7,7.,1.8));
#12006=CARTESIAN_POINT('',(2.1,7.,1.8));
#12007=CARTESIAN_POINT('Origin',(2.7,7.,1.8));
#12008=CARTESIAN_POINT('',(2.1,7.,1.8));
#12009=CARTESIAN_POINT('Origin',(2.7,7.,3.42222222222222));
#12010=CARTESIAN_POINT('Origin',(2.7,7.,1.8));
#12011=CARTESIAN_POINT('',(2.37,7.,1.8));
#12012=CARTESIAN_POINT('Origin',(2.7,7.,1.8));
#12013=CARTESIAN_POINT('Origin',(-2.7,7.,0.9));
#12014=CARTESIAN_POINT('',(-3.03,7.,1.));
#12015=CARTESIAN_POINT('Origin',(-2.7,7.,1.));
#12016=CARTESIAN_POINT('',(-3.03,7.,0.9));
#12017=CARTESIAN_POINT('Origin',(2.7,7.,0.9));
#12018=CARTESIAN_POINT('',(2.37,7.,1.));
#12019=CARTESIAN_POINT('Origin',(2.7,7.,1.));
#12020=CARTESIAN_POINT('',(2.37,7.,0.9));
#12021=CARTESIAN_POINT('Origin',(1.7,6.2,5.2));
#12022=CARTESIAN_POINT('',(1.71218189678592,6.2,5.17834329460281));
#12023=CARTESIAN_POINT('',(1.71218189678592,7.8,5.17834329460281));
#12024=CARTESIAN_POINT('',(1.71218189678592,6.2,5.17834329460281));
#12025=CARTESIAN_POINT('',(3.5,6.2,2.));
#12026=CARTESIAN_POINT('',(3.5,6.2,2.));
#12027=CARTESIAN_POINT('',(3.5,7.8,2.));
#12028=CARTESIAN_POINT('',(3.5,6.2,2.));
#12029=CARTESIAN_POINT('',(3.5,7.8,2.));
#12030=CARTESIAN_POINT('Origin',(-3.5,6.2,2.));
#12031=CARTESIAN_POINT('',(-1.71218189678592,7.8,5.17834329460281));
#12032=CARTESIAN_POINT('',(-1.71218189678592,6.2,5.17834329460281));
#12033=CARTESIAN_POINT('',(-1.71218189678592,6.2,5.17834329460281));
#12034=CARTESIAN_POINT('',(-3.5,7.8,2.));
#12035=CARTESIAN_POINT('',(-1.7,7.8,5.2));
#12036=CARTESIAN_POINT('',(-3.5,6.2,2.));
#12037=CARTESIAN_POINT('',(-3.5,6.2,2.));
#12038=CARTESIAN_POINT('',(-1.7,6.2,5.2));
#12039=CARTESIAN_POINT('Origin',(-3.5,6.2,1.));
#12040=CARTESIAN_POINT('',(-3.5,6.2,1.));
#12041=CARTESIAN_POINT('',(-3.5,6.2,2.));
#12042=CARTESIAN_POINT('',(-3.5,7.8,1.));
#12043=CARTESIAN_POINT('',(-3.5,7.8,2.));
#12044=CARTESIAN_POINT('',(-3.5,6.2,1.));
#12045=CARTESIAN_POINT('Origin',(3.5,6.2,1.));
#12046=CARTESIAN_POINT('',(3.5,6.2,1.));
#12047=CARTESIAN_POINT('',(-3.5,6.2,1.));
#12048=CARTESIAN_POINT('',(3.5,7.8,1.));
#12049=CARTESIAN_POINT('',(-3.5,7.8,1.));
#12050=CARTESIAN_POINT('',(3.5,6.2,1.));
#12051=CARTESIAN_POINT('Origin',(3.5,6.2,2.));
#12052=CARTESIAN_POINT('',(3.5,6.2,1.));
#12053=CARTESIAN_POINT('',(3.5,7.8,1.));
#12054=CARTESIAN_POINT('Origin',(0.,7.8,7.));
#12055=CARTESIAN_POINT('Origin',(0.,7.8,7.));
#12056=CARTESIAN_POINT('',(-1.6,7.8,7.));
#12057=CARTESIAN_POINT('Origin',(0.,7.8,7.));
#12058=CARTESIAN_POINT('Origin',(0.,6.2,7.));
#12059=CARTESIAN_POINT('',(-1.6,6.2,7.));
#12060=CARTESIAN_POINT('',(-1.6,6.2,7.));
#12061=CARTESIAN_POINT('Origin',(0.,6.2,7.));
#12062=CARTESIAN_POINT('Origin',(0.,6.2,7.));
#12063=CARTESIAN_POINT('Origin',(0.,6.2,7.));
#12064=CARTESIAN_POINT('Origin',(0.,6.2,7.));
#12065=CARTESIAN_POINT('',(0.,0.,0.));
#12066=CARTESIAN_POINT('Origin',(-2.,5.8,7.));
#12067=CARTESIAN_POINT('',(-2.225,5.9,7.));
#12068=CARTESIAN_POINT('Origin',(-2.,5.9,7.));
#12069=CARTESIAN_POINT('',(-2.225,6.2,7.));
#12070=CARTESIAN_POINT('',(-2.225,5.8,7.));
#12071=CARTESIAN_POINT('Origin',(-2.,6.2,7.));
#12072=CARTESIAN_POINT('Origin',(1.22464679914735E-16,5.8,9.));
#12073=CARTESIAN_POINT('',(-0.225,5.9,9.));
#12074=CARTESIAN_POINT('Origin',(1.22464679914735E-16,5.9,9.));
#12075=CARTESIAN_POINT('',(-0.225,6.2,9.));
#12076=CARTESIAN_POINT('',(-0.225,5.8,9.));
#12077=CARTESIAN_POINT('Origin',(1.22464679914735E-16,6.2,9.));
#12078=CARTESIAN_POINT('Origin',(2.,5.8,7.));
#12079=CARTESIAN_POINT('',(1.775,5.9,7.));
#12080=CARTESIAN_POINT('Origin',(2.,5.9,7.));
#12081=CARTESIAN_POINT('',(1.775,6.2,7.));
#12082=CARTESIAN_POINT('',(1.775,5.8,7.));
#12083=CARTESIAN_POINT('Origin',(2.,6.2,7.));
#12084=CARTESIAN_POINT('Origin',(-3.67394039744206E-16,5.8,5.));
#12085=CARTESIAN_POINT('',(-0.225,5.9,5.));
#12086=CARTESIAN_POINT('Origin',(-3.67394039744206E-16,5.9,5.));
#12087=CARTESIAN_POINT('',(-0.225,6.2,5.));
#12088=CARTESIAN_POINT('',(-0.225,5.8,5.));
#12089=CARTESIAN_POINT('Origin',(-3.67394039744206E-16,6.2,5.));
#12090=CARTESIAN_POINT('Origin',(0.,6.2,7.));
#12091=CARTESIAN_POINT('',(-1.59,6.5,7.));
#12092=CARTESIAN_POINT('Origin',(0.,6.5,7.));
#12093=CARTESIAN_POINT('',(-1.59,6.2,7.));
#12094=CARTESIAN_POINT('',(-1.59,6.2,7.));
#12095=CARTESIAN_POINT('Origin',(0.,6.2,7.));
#12096=CARTESIAN_POINT('Origin',(0.,6.5,7.));
#12097=CARTESIAN_POINT('',(-1.1,6.5,7.));
#12098=CARTESIAN_POINT('Origin',(0.,6.5,7.));
#12099=CARTESIAN_POINT('Origin',(0.,5.9,7.));
#12100=CARTESIAN_POINT('',(-1.1,5.9,7.));
#12101=CARTESIAN_POINT('',(-1.1,5.9,7.));
#12102=CARTESIAN_POINT('Origin',(0.,5.9,7.));
#12103=CARTESIAN_POINT('Origin',(0.,5.9,7.));
#12104=CARTESIAN_POINT('',(-2.5,6.2,7.));
#12105=CARTESIAN_POINT('Origin',(0.,6.2,7.));
#12106=CARTESIAN_POINT('',(-2.5,5.9,7.));
#12107=CARTESIAN_POINT('',(-2.5,5.9,7.));
#12108=CARTESIAN_POINT('Origin',(0.,5.9,7.));
#12109=CARTESIAN_POINT('Origin',(0.,6.2,7.));
#12110=CARTESIAN_POINT('Origin',(0.,5.9,7.));
#12111=CARTESIAN_POINT('',(0.,0.,0.));
#12112=CARTESIAN_POINT('Origin',(-2.,7.7,7.));
#12113=CARTESIAN_POINT('',(-2.225,7.8,7.));
#12114=CARTESIAN_POINT('Origin',(-2.,7.8,7.));
#12115=CARTESIAN_POINT('',(-2.225,8.1,7.));
#12116=CARTESIAN_POINT('',(-2.225,7.7,7.));
#12117=CARTESIAN_POINT('Origin',(-2.,8.1,7.));
#12118=CARTESIAN_POINT('Origin',(1.22464679914735E-16,7.7,9.));
#12119=CARTESIAN_POINT('',(-0.225,7.8,9.));
#12120=CARTESIAN_POINT('Origin',(1.22464679914735E-16,7.8,9.));
#12121=CARTESIAN_POINT('',(-0.225,8.1,9.));
#12122=CARTESIAN_POINT('',(-0.225,7.7,9.));
#12123=CARTESIAN_POINT('Origin',(1.22464679914735E-16,8.1,9.));
#12124=CARTESIAN_POINT('Origin',(2.,7.7,7.));
#12125=CARTESIAN_POINT('',(1.775,7.8,7.));
#12126=CARTESIAN_POINT('Origin',(2.,7.8,7.));
#12127=CARTESIAN_POINT('',(1.775,8.1,7.));
#12128=CARTESIAN_POINT('',(1.775,7.7,7.));
#12129=CARTESIAN_POINT('Origin',(2.,8.1,7.));
#12130=CARTESIAN_POINT('Origin',(-3.67394039744206E-16,7.7,5.));
#12131=CARTESIAN_POINT('',(-0.225,7.8,5.));
#12132=CARTESIAN_POINT('Origin',(-3.67394039744206E-16,7.8,5.));
#12133=CARTESIAN_POINT('',(-0.225,8.1,5.));
#12134=CARTESIAN_POINT('',(-0.225,7.7,5.));
#12135=CARTESIAN_POINT('Origin',(-3.67394039744206E-16,8.1,5.));
#12136=CARTESIAN_POINT('Origin',(0.,7.5,7.));
#12137=CARTESIAN_POINT('',(-1.59,7.8,7.));
#12138=CARTESIAN_POINT('Origin',(0.,7.8,7.));
#12139=CARTESIAN_POINT('',(-1.59,7.5,7.));
#12140=CARTESIAN_POINT('',(-1.59,7.5,7.));
#12141=CARTESIAN_POINT('Origin',(0.,7.5,7.));
#12142=CARTESIAN_POINT('Origin',(0.,7.5,7.));
#12143=CARTESIAN_POINT('',(-1.1,7.5,7.));
#12144=CARTESIAN_POINT('Origin',(0.,7.5,7.));
#12145=CARTESIAN_POINT('Origin',(0.,7.8,7.));
#12146=CARTESIAN_POINT('',(-1.1,8.1,7.));
#12147=CARTESIAN_POINT('Origin',(0.,8.1,7.));
#12148=CARTESIAN_POINT('',(-1.1,7.8,7.));
#12149=CARTESIAN_POINT('Origin',(0.,7.8,7.));
#12150=CARTESIAN_POINT('',(-2.5,8.1,7.));
#12151=CARTESIAN_POINT('Origin',(0.,8.1,7.));
#12152=CARTESIAN_POINT('',(-2.5,7.8,7.));
#12153=CARTESIAN_POINT('',(-2.5,7.8,7.));
#12154=CARTESIAN_POINT('Origin',(0.,7.8,7.));
#12155=CARTESIAN_POINT('Origin',(0.,8.1,7.));
#12156=CARTESIAN_POINT('Origin',(0.,7.8,7.));
#12157=CARTESIAN_POINT('',(0.,0.,0.));
#12158=CARTESIAN_POINT('Origin',(-1.83847763108502,-0.9,5.16152236891498));
#12159=CARTESIAN_POINT('',(-2.00347763108502,-0.8,5.16152236891498));
#12160=CARTESIAN_POINT('Origin',(-1.83847763108502,-0.8,5.16152236891498));
#12161=CARTESIAN_POINT('',(-2.00347763108502,0.8,5.16152236891498));
#12162=CARTESIAN_POINT('',(-2.00347763108502,-0.9,5.16152236891498));
#12163=CARTESIAN_POINT('Origin',(-1.83847763108502,0.8,5.16152236891498));
#12164=CARTESIAN_POINT('Origin',(-1.83847763108502,-0.9,8.83847763108502));
#12165=CARTESIAN_POINT('',(-2.00347763108502,-0.8,8.83847763108502));
#12166=CARTESIAN_POINT('Origin',(-1.83847763108502,-0.8,8.83847763108502));
#12167=CARTESIAN_POINT('',(-2.00347763108502,0.8,8.83847763108502));
#12168=CARTESIAN_POINT('',(-2.00347763108502,-0.9,8.83847763108502));
#12169=CARTESIAN_POINT('Origin',(-1.83847763108502,0.8,8.83847763108502));
#12170=CARTESIAN_POINT('Origin',(1.83847763108502,-0.9,8.83847763108502));
#12171=CARTESIAN_POINT('',(1.67347763108502,-0.8,8.83847763108502));
#12172=CARTESIAN_POINT('Origin',(1.83847763108502,-0.8,8.83847763108502));
#12173=CARTESIAN_POINT('',(1.67347763108502,0.8,8.83847763108502));
#12174=CARTESIAN_POINT('',(1.67347763108502,-0.9,8.83847763108502));
#12175=CARTESIAN_POINT('Origin',(1.83847763108502,0.8,8.83847763108502));
#12176=CARTESIAN_POINT('Origin',(1.83847763108502,-0.9,5.16152236891498));
#12177=CARTESIAN_POINT('',(1.67347763108502,-0.8,5.16152236891498));
#12178=CARTESIAN_POINT('Origin',(1.83847763108502,-0.8,5.16152236891498));
#12179=CARTESIAN_POINT('',(1.67347763108502,0.8,5.16152236891498));
#12180=CARTESIAN_POINT('',(1.67347763108502,-0.9,5.16152236891498));
#12181=CARTESIAN_POINT('Origin',(1.83847763108502,0.8,5.16152236891498));
#12182=CARTESIAN_POINT('Origin',(10.,-0.5,6.5));
#12183=CARTESIAN_POINT('',(2.95803989154981,0.5,6.5));
#12184=CARTESIAN_POINT('',(2.95803989154981,-0.5,6.5));
#12185=CARTESIAN_POINT('',(2.95803989154981,-0.8,6.5));
#12186=CARTESIAN_POINT('',(10.,0.5,6.5));
#12187=CARTESIAN_POINT('',(2.,0.5,6.5));
#12188=CARTESIAN_POINT('',(10.,-0.5,6.5));
#12189=CARTESIAN_POINT('',(10.,-0.5,6.5));
#12190=CARTESIAN_POINT('',(2.,-0.5,6.5));
#12191=CARTESIAN_POINT('Origin',(6.,0.5,7.));
#12192=CARTESIAN_POINT('',(2.95803989154981,0.5,7.5));
#12193=CARTESIAN_POINT('Origin',(0.,0.5,7.));
#12194=CARTESIAN_POINT('',(10.,0.5,7.5));
#12195=CARTESIAN_POINT('',(10.,0.5,7.5));
#12196=CARTESIAN_POINT('',(10.,0.5,6.5));
#12197=CARTESIAN_POINT('Origin',(6.,-0.5,7.));
#12198=CARTESIAN_POINT('',(2.95803989154981,-0.5,7.5));
#12199=CARTESIAN_POINT('Origin',(0.,-0.5,7.));
#12200=CARTESIAN_POINT('',(10.,-0.5,7.5));
#12201=CARTESIAN_POINT('',(10.,-0.5,6.5));
#12202=CARTESIAN_POINT('',(10.,-0.5,7.5));
#12203=CARTESIAN_POINT('Origin',(2.,-0.5,7.5));
#12204=CARTESIAN_POINT('',(2.95803989154981,-0.8,7.5));
#12205=CARTESIAN_POINT('',(10.,-0.5,7.5));
#12206=CARTESIAN_POINT('Origin',(10.,-0.5,7.5));
#12207=CARTESIAN_POINT('Origin',(0.,-0.8,7.));
#12208=CARTESIAN_POINT('',(-2.35,0.8,7.));
#12209=CARTESIAN_POINT('Origin',(0.,0.8,7.));
#12210=CARTESIAN_POINT('',(-2.35,-0.8,7.));
#12211=CARTESIAN_POINT('',(-2.35,-0.8,7.));
#12212=CARTESIAN_POINT('Origin',(0.,-0.8,7.));
#12213=CARTESIAN_POINT('Origin',(0.,-0.8,7.));
#12214=CARTESIAN_POINT('',(-3.,0.8,7.));
#12215=CARTESIAN_POINT('Origin',(0.,0.8,7.));
#12216=CARTESIAN_POINT('',(-3.,-0.8,7.));
#12217=CARTESIAN_POINT('',(-3.,-0.8,7.));
#12218=CARTESIAN_POINT('Origin',(0.,-0.8,7.));
#12219=CARTESIAN_POINT('Origin',(0.,0.8,7.));
#12220=CARTESIAN_POINT('Origin',(0.,-0.8,7.));
#12221=CARTESIAN_POINT('',(0.,0.,0.));
#12222=CARTESIAN_POINT('Origin',(-1.83847763108502,-1.2,5.16152236891498));
#12223=CARTESIAN_POINT('',(-2.06347763108502,-1.1,5.16152236891498));
#12224=CARTESIAN_POINT('Origin',(-1.83847763108502,-1.1,5.16152236891498));
#12225=CARTESIAN_POINT('',(-2.06347763108502,-0.8,5.16152236891498));
#12226=CARTESIAN_POINT('',(-2.06347763108502,-1.2,5.16152236891498));
#12227=CARTESIAN_POINT('Origin',(-1.83847763108502,-0.8,5.16152236891498));
#12228=CARTESIAN_POINT('Origin',(-1.83847763108502,-1.2,8.83847763108502));
#12229=CARTESIAN_POINT('',(-2.06347763108502,-1.1,8.83847763108502));
#12230=CARTESIAN_POINT('Origin',(-1.83847763108502,-1.1,8.83847763108502));
#12231=CARTESIAN_POINT('',(-2.06347763108502,-0.8,8.83847763108502));
#12232=CARTESIAN_POINT('',(-2.06347763108502,-1.2,8.83847763108502));
#12233=CARTESIAN_POINT('Origin',(-1.83847763108502,-0.8,8.83847763108502));
#12234=CARTESIAN_POINT('Origin',(1.83847763108502,-1.2,8.83847763108502));
#12235=CARTESIAN_POINT('',(1.61347763108502,-1.1,8.83847763108502));
#12236=CARTESIAN_POINT('Origin',(1.83847763108502,-1.1,8.83847763108502));
#12237=CARTESIAN_POINT('',(1.61347763108502,-0.8,8.83847763108502));
#12238=CARTESIAN_POINT('',(1.61347763108502,-1.2,8.83847763108502));
#12239=CARTESIAN_POINT('Origin',(1.83847763108502,-0.8,8.83847763108502));
#12240=CARTESIAN_POINT('Origin',(1.83847763108502,-1.2,5.16152236891498));
#12241=CARTESIAN_POINT('',(1.61347763108502,-1.1,5.16152236891498));
#12242=CARTESIAN_POINT('Origin',(1.83847763108502,-1.1,5.16152236891498));
#12243=CARTESIAN_POINT('',(1.61347763108502,-0.8,5.16152236891498));
#12244=CARTESIAN_POINT('',(1.61347763108502,-1.2,5.16152236891498));
#12245=CARTESIAN_POINT('Origin',(1.83847763108502,-0.8,5.16152236891498));
#12246=CARTESIAN_POINT('Origin',(0.,-0.8,7.));
#12247=CARTESIAN_POINT('',(-2.34,-0.7,7.));
#12248=CARTESIAN_POINT('Origin',(0.,-0.7,7.));
#12249=CARTESIAN_POINT('',(-2.34,-0.8,7.));
#12250=CARTESIAN_POINT('',(-2.34,-0.8,7.));
#12251=CARTESIAN_POINT('Origin',(0.,-0.8,7.));
#12252=CARTESIAN_POINT('Origin',(0.,-0.7,7.));
#12253=CARTESIAN_POINT('',(-1.9,-0.7,7.));
#12254=CARTESIAN_POINT('Origin',(0.,-0.7,7.));
#12255=CARTESIAN_POINT('Origin',(0.,-1.1,7.));
#12256=CARTESIAN_POINT('',(-1.9,-1.1,7.));
#12257=CARTESIAN_POINT('',(-1.9,-1.1,7.));
#12258=CARTESIAN_POINT('Origin',(0.,-1.1,7.));
#12259=CARTESIAN_POINT('Origin',(0.,-1.1,7.));
#12260=CARTESIAN_POINT('',(-3.,-0.8,7.));
#12261=CARTESIAN_POINT('Origin',(0.,-0.8,7.));
#12262=CARTESIAN_POINT('',(-3.,-1.1,7.));
#12263=CARTESIAN_POINT('',(-3.,-1.1,7.));
#12264=CARTESIAN_POINT('Origin',(0.,-1.1,7.));
#12265=CARTESIAN_POINT('Origin',(0.,-0.8,7.));
#12266=CARTESIAN_POINT('Origin',(0.,-1.1,7.));
#12267=CARTESIAN_POINT('',(0.,0.,0.));
#12268=CARTESIAN_POINT('Origin',(-1.83847763108502,0.7,5.16152236891498));
#12269=CARTESIAN_POINT('',(-2.06347763108502,0.8,5.16152236891498));
#12270=CARTESIAN_POINT('Origin',(-1.83847763108502,0.8,5.16152236891498));
#12271=CARTESIAN_POINT('',(-2.06347763108502,1.1,5.16152236891498));
#12272=CARTESIAN_POINT('',(-2.06347763108502,0.7,5.16152236891498));
#12273=CARTESIAN_POINT('Origin',(-1.83847763108502,1.1,5.16152236891498));
#12274=CARTESIAN_POINT('Origin',(-1.83847763108502,0.7,8.83847763108502));
#12275=CARTESIAN_POINT('',(-2.06347763108502,0.8,8.83847763108502));
#12276=CARTESIAN_POINT('Origin',(-1.83847763108502,0.8,8.83847763108502));
#12277=CARTESIAN_POINT('',(-2.06347763108502,1.1,8.83847763108502));
#12278=CARTESIAN_POINT('',(-2.06347763108502,0.7,8.83847763108502));
#12279=CARTESIAN_POINT('Origin',(-1.83847763108502,1.1,8.83847763108502));
#12280=CARTESIAN_POINT('Origin',(1.83847763108502,0.7,8.83847763108502));
#12281=CARTESIAN_POINT('',(1.61347763108502,0.8,8.83847763108502));
#12282=CARTESIAN_POINT('Origin',(1.83847763108502,0.8,8.83847763108502));
#12283=CARTESIAN_POINT('',(1.61347763108502,1.1,8.83847763108502));
#12284=CARTESIAN_POINT('',(1.61347763108502,0.7,8.83847763108502));
#12285=CARTESIAN_POINT('Origin',(1.83847763108502,1.1,8.83847763108502));
#12286=CARTESIAN_POINT('Origin',(1.83847763108502,0.7,5.16152236891498));
#12287=CARTESIAN_POINT('',(1.61347763108502,0.8,5.16152236891498));
#12288=CARTESIAN_POINT('Origin',(1.83847763108502,0.8,5.16152236891498));
#12289=CARTESIAN_POINT('',(1.61347763108502,1.1,5.16152236891498));
#12290=CARTESIAN_POINT('',(1.61347763108502,0.7,5.16152236891498));
#12291=CARTESIAN_POINT('Origin',(1.83847763108502,1.1,5.16152236891498));
#12292=CARTESIAN_POINT('Origin',(0.,0.7,7.));
#12293=CARTESIAN_POINT('',(-2.34,0.8,7.));
#12294=CARTESIAN_POINT('Origin',(0.,0.8,7.));
#12295=CARTESIAN_POINT('',(-2.34,0.7,7.));
#12296=CARTESIAN_POINT('',(-2.34,0.7,7.));
#12297=CARTESIAN_POINT('Origin',(0.,0.7,7.));
#12298=CARTESIAN_POINT('Origin',(0.,0.7,7.));
#12299=CARTESIAN_POINT('',(-1.9,0.7,7.));
#12300=CARTESIAN_POINT('Origin',(0.,0.7,7.));
#12301=CARTESIAN_POINT('Origin',(0.,0.8,7.));
#12302=CARTESIAN_POINT('',(-1.9,1.1,7.));
#12303=CARTESIAN_POINT('Origin',(0.,1.1,7.));
#12304=CARTESIAN_POINT('',(-1.9,0.8,7.));
#12305=CARTESIAN_POINT('Origin',(0.,0.8,7.));
#12306=CARTESIAN_POINT('',(-3.,1.1,7.));
#12307=CARTESIAN_POINT('Origin',(0.,1.1,7.));
#12308=CARTESIAN_POINT('',(-3.,0.8,7.));
#12309=CARTESIAN_POINT('',(-3.,0.8,7.));
#12310=CARTESIAN_POINT('Origin',(0.,0.8,7.));
#12311=CARTESIAN_POINT('Origin',(0.,1.1,7.));
#12312=CARTESIAN_POINT('Origin',(0.,0.8,7.));
#12313=CARTESIAN_POINT('',(0.,0.,0.));
#12314=CARTESIAN_POINT('Origin',(10.,-1.7,3.5));
#12315=CARTESIAN_POINT('',(9.835,-1.7,3.5));
#12316=CARTESIAN_POINT('Origin',(10.,-1.7,3.5));
#12317=CARTESIAN_POINT('',(9.835,-1.7,4.5));
#12318=CARTESIAN_POINT('',(9.835,-1.7,3.5));
#12319=CARTESIAN_POINT('Origin',(10.,-1.7,4.5));
#12320=CARTESIAN_POINT('Origin',(10.,-1.7,3.5));
#12321=CARTESIAN_POINT('Origin',(10.,1.7,3.5));
#12322=CARTESIAN_POINT('',(9.835,1.7,3.5));
#12323=CARTESIAN_POINT('Origin',(10.,1.7,3.5));
#12324=CARTESIAN_POINT('',(9.835,1.7,4.5));
#12325=CARTESIAN_POINT('',(9.835,1.7,3.5));
#12326=CARTESIAN_POINT('Origin',(10.,1.7,4.5));
#12327=CARTESIAN_POINT('Origin',(10.,1.7,3.5));
#12328=CARTESIAN_POINT('Origin',(11.4,-1.4,2.2));
#12329=CARTESIAN_POINT('',(10.9,-1.4,2.2));
#12330=CARTESIAN_POINT('Origin',(11.4,-1.4,2.2));
#12331=CARTESIAN_POINT('',(10.9,-1.4,4.5));
#12332=CARTESIAN_POINT('',(10.9,-1.4,2.2));
#12333=CARTESIAN_POINT('Origin',(11.4,-1.4,4.5));
#12334=CARTESIAN_POINT('Origin',(11.4,-1.4,2.2));
#12335=CARTESIAN_POINT('',(11.125,-1.4,2.2));
#12336=CARTESIAN_POINT('Origin',(11.4,-1.4,2.2));
#12337=CARTESIAN_POINT('Origin',(8.6,1.4,2.2));
#12338=CARTESIAN_POINT('',(8.1,1.4,2.2));
#12339=CARTESIAN_POINT('Origin',(8.6,1.4,2.2));
#12340=CARTESIAN_POINT('',(8.1,1.4,4.5));
#12341=CARTESIAN_POINT('',(8.1,1.4,2.2));
#12342=CARTESIAN_POINT('Origin',(8.6,1.4,4.5));
#12343=CARTESIAN_POINT('Origin',(8.6,1.4,2.2));
#12344=CARTESIAN_POINT('',(8.325,1.4,2.2));
#12345=CARTESIAN_POINT('Origin',(8.6,1.4,2.2));
#12346=CARTESIAN_POINT('Origin',(8.6,-1.4,2.2));
#12347=CARTESIAN_POINT('',(8.1,-1.4,2.2));
#12348=CARTESIAN_POINT('Origin',(8.6,-1.4,2.2));
#12349=CARTESIAN_POINT('',(8.1,-1.4,4.5));
#12350=CARTESIAN_POINT('',(8.1,-1.4,2.2));
#12351=CARTESIAN_POINT('Origin',(8.6,-1.4,4.5));
#12352=CARTESIAN_POINT('Origin',(8.6,-1.4,2.2));
#12353=CARTESIAN_POINT('',(8.325,-1.4,2.2));
#12354=CARTESIAN_POINT('Origin',(8.6,-1.4,2.2));
#12355=CARTESIAN_POINT('Origin',(11.4,1.4,2.2));
#12356=CARTESIAN_POINT('',(10.9,1.4,2.2));
#12357=CARTESIAN_POINT('Origin',(11.4,1.4,2.2));
#12358=CARTESIAN_POINT('',(10.9,1.4,4.5));
#12359=CARTESIAN_POINT('',(10.9,1.4,2.2));
#12360=CARTESIAN_POINT('Origin',(11.4,1.4,4.5));
#12361=CARTESIAN_POINT('Origin',(11.4,1.4,2.2));
#12362=CARTESIAN_POINT('',(11.125,1.4,2.2));
#12363=CARTESIAN_POINT('Origin',(11.4,1.4,2.2));
#12364=CARTESIAN_POINT('Origin',(11.4,-1.4,0.9));
#12365=CARTESIAN_POINT('',(11.125,-1.4,1.));
#12366=CARTESIAN_POINT('Origin',(11.4,-1.4,1.));
#12367=CARTESIAN_POINT('',(11.125,-1.4,0.9));
#12368=CARTESIAN_POINT('Origin',(8.6,1.4,0.9));
#12369=CARTESIAN_POINT('',(8.325,1.4,1.));
#12370=CARTESIAN_POINT('Origin',(8.6,1.4,1.));
#12371=CARTESIAN_POINT('',(8.325,1.4,0.9));
#12372=CARTESIAN_POINT('Origin',(8.6,-1.4,0.9));
#12373=CARTESIAN_POINT('',(8.325,-1.4,1.));
#12374=CARTESIAN_POINT('Origin',(8.6,-1.4,1.));
#12375=CARTESIAN_POINT('',(8.325,-1.4,0.9));
#12376=CARTESIAN_POINT('Origin',(11.4,1.4,0.9));
#12377=CARTESIAN_POINT('',(11.125,1.4,1.));
#12378=CARTESIAN_POINT('Origin',(11.4,1.4,1.));
#12379=CARTESIAN_POINT('',(11.125,1.4,0.9));
#12380=CARTESIAN_POINT('Origin',(12.,2.,1.));
#12381=CARTESIAN_POINT('',(12.,2.,1.));
#12382=CARTESIAN_POINT('',(8.,2.,1.));
#12383=CARTESIAN_POINT('',(12.,2.,1.));
#12384=CARTESIAN_POINT('',(8.,2.,4.5));
#12385=CARTESIAN_POINT('',(8.,2.,1.));
#12386=CARTESIAN_POINT('',(12.,2.,4.5));
#12387=CARTESIAN_POINT('',(12.,2.,4.5));
#12388=CARTESIAN_POINT('',(12.,2.,1.));
#12389=CARTESIAN_POINT('Origin',(12.,-2.,1.));
#12390=CARTESIAN_POINT('',(12.,-2.,1.));
#12391=CARTESIAN_POINT('',(12.,-2.,1.));
#12392=CARTESIAN_POINT('',(12.,-2.,4.5));
#12393=CARTESIAN_POINT('',(12.,-2.,4.5));
#12394=CARTESIAN_POINT('',(12.,-2.,1.));
#12395=CARTESIAN_POINT('Origin',(8.,-2.,1.));
#12396=CARTESIAN_POINT('',(8.,-2.,1.));
#12397=CARTESIAN_POINT('',(8.,-2.,1.));
#12398=CARTESIAN_POINT('',(8.,-2.,4.5));
#12399=CARTESIAN_POINT('',(8.,-2.,4.5));
#12400=CARTESIAN_POINT('',(8.,-2.,1.));
#12401=CARTESIAN_POINT('Origin',(8.,2.,1.));
#12402=CARTESIAN_POINT('',(8.,2.,1.));
#12403=CARTESIAN_POINT('',(8.,2.,4.5));
#12404=CARTESIAN_POINT('Origin',(10.,0.,4.5));
#12405=CARTESIAN_POINT('Origin',(10.,0.,1.));
#12406=CARTESIAN_POINT('',(0.,0.,0.));
#12407=CARTESIAN_POINT('Origin',(10.,-1.7,4.4));
#12408=CARTESIAN_POINT('',(9.775,-1.7,4.5));
#12409=CARTESIAN_POINT('Origin',(10.,-1.7,4.5));
#12410=CARTESIAN_POINT('',(9.775,-1.7,4.9));
#12411=CARTESIAN_POINT('',(9.775,-1.7,4.4));
#12412=CARTESIAN_POINT('Origin',(10.,-1.7,4.9));
#12413=CARTESIAN_POINT('Origin',(10.,1.7,4.4));
#12414=CARTESIAN_POINT('',(9.775,1.7,4.5));
#12415=CARTESIAN_POINT('Origin',(10.,1.7,4.5));
#12416=CARTESIAN_POINT('',(9.775,1.7,4.9));
#12417=CARTESIAN_POINT('',(9.775,1.7,4.4));
#12418=CARTESIAN_POINT('Origin',(10.,1.7,4.9));
#12419=CARTESIAN_POINT('Origin',(9.,1.2,4.9));
#12420=CARTESIAN_POINT('',(11.,1.2,4.9));
#12421=CARTESIAN_POINT('',(9.,1.2,4.9));
#12422=CARTESIAN_POINT('',(10.,1.2,4.9));
#12423=CARTESIAN_POINT('',(11.,2.2,4.9));
#12424=CARTESIAN_POINT('',(11.,1.2,4.9));
#12425=CARTESIAN_POINT('',(9.,2.2,4.9));
#12426=CARTESIAN_POINT('',(11.,2.2,4.9));
#12427=CARTESIAN_POINT('',(9.,1.2,4.9));
#12428=CARTESIAN_POINT('Origin',(10.,2.2,4.7));
#12429=CARTESIAN_POINT('',(11.,2.2,4.5));
#12430=CARTESIAN_POINT('',(11.,2.2,4.5));
#12431=CARTESIAN_POINT('',(9.,2.2,4.5));
#12432=CARTESIAN_POINT('',(9.,2.2,4.5));
#12433=CARTESIAN_POINT('',(9.,2.2,4.9));
#12434=CARTESIAN_POINT('Origin',(11.,1.2,4.5));
#12435=CARTESIAN_POINT('',(9.,1.2,6.5));
#12436=CARTESIAN_POINT('',(9.,1.2,4.5));
#12437=CARTESIAN_POINT('',(11.,1.2,6.5));
#12438=CARTESIAN_POINT('',(11.,1.2,6.5));
#12439=CARTESIAN_POINT('',(11.,1.2,4.5));
#12440=CARTESIAN_POINT('Origin',(9.,-2.2,4.9));
#12441=CARTESIAN_POINT('',(11.,-2.2,4.9));
#12442=CARTESIAN_POINT('',(9.,-2.2,4.9));
#12443=CARTESIAN_POINT('',(11.,-2.2,4.9));
#12444=CARTESIAN_POINT('',(11.,-1.2,4.9));
#12445=CARTESIAN_POINT('',(11.,-2.2,4.9));
#12446=CARTESIAN_POINT('',(9.,-1.2,4.9));
#12447=CARTESIAN_POINT('',(9.,-1.2,4.9));
#12448=CARTESIAN_POINT('',(9.,-2.2,4.9));
#12449=CARTESIAN_POINT('Origin',(10.,-2.2,4.7));
#12450=CARTESIAN_POINT('',(9.,-2.2,4.5));
#12451=CARTESIAN_POINT('',(9.,-2.2,4.9));
#12452=CARTESIAN_POINT('',(11.,-2.2,4.5));
#12453=CARTESIAN_POINT('',(9.,-2.2,4.5));
#12454=CARTESIAN_POINT('',(11.,-2.2,4.5));
#12455=CARTESIAN_POINT('Origin',(11.,-1.2,4.5));
#12456=CARTESIAN_POINT('',(11.,-2.2,4.5));
#12457=CARTESIAN_POINT('',(11.,-1.2,6.5));
#12458=CARTESIAN_POINT('',(11.,-1.2,6.5));
#12459=CARTESIAN_POINT('',(11.,-1.2,4.5));
#12460=CARTESIAN_POINT('Origin',(9.,-1.2,4.5));
#12461=CARTESIAN_POINT('',(9.,-1.2,6.5));
#12462=CARTESIAN_POINT('',(9.,-1.2,6.5));
#12463=CARTESIAN_POINT('',(9.,-1.2,4.5));
#12464=CARTESIAN_POINT('Origin',(9.,1.2,4.5));
#12465=CARTESIAN_POINT('',(9.,1.2,4.5));
#12466=CARTESIAN_POINT('',(9.,1.2,6.5));
#12467=CARTESIAN_POINT('Origin',(10.,0.,6.5));
#12468=CARTESIAN_POINT('Origin',(10.,0.,4.5));
#12469=CARTESIAN_POINT('',(0.,0.,0.));
#12470=CARTESIAN_POINT('Origin',(4.4,3.4,1.5));
#12471=CARTESIAN_POINT('',(4.,3.4,1.5));
#12472=CARTESIAN_POINT('Origin',(4.4,3.4,1.5));
#12473=CARTESIAN_POINT('',(4.,3.4,11.5));
#12474=CARTESIAN_POINT('',(4.,3.4,1.5));
#12475=CARTESIAN_POINT('Origin',(4.4,3.4,11.5));
#12476=CARTESIAN_POINT('Origin',(4.4,3.4,1.5));
#12477=CARTESIAN_POINT('',(4.175,3.4,1.5));
#12478=CARTESIAN_POINT('Origin',(4.4,3.4,1.5));
#12479=CARTESIAN_POINT('Origin',(4.4,3.4,0.9));
#12480=CARTESIAN_POINT('',(4.175,3.4,1.));
#12481=CARTESIAN_POINT('Origin',(4.4,3.4,1.));
#12482=CARTESIAN_POINT('',(4.175,3.4,0.9));
#12483=CARTESIAN_POINT('Origin',(4.4,3.4,1.5));
#12484=CARTESIAN_POINT('',(3.5,3.4,1.5));
#12485=CARTESIAN_POINT('Origin',(4.4,3.4,1.5));
#12486=CARTESIAN_POINT('',(3.8,4.,1.5));
#12487=CARTESIAN_POINT('',(3.8,2.8,1.5));
#12488=CARTESIAN_POINT('',(3.8,3.1,1.5));
#12489=CARTESIAN_POINT('',(5.,4.,1.5));
#12490=CARTESIAN_POINT('',(4.7,4.,1.5));
#12491=CARTESIAN_POINT('',(5.,2.8,1.5));
#12492=CARTESIAN_POINT('',(5.,-0.3,1.5));
#12493=CARTESIAN_POINT('',(4.4,2.8,1.5));
#12494=CARTESIAN_POINT('Origin',(4.4,3.4,1.));
#12495=CARTESIAN_POINT('',(3.5,3.4,1.));
#12496=CARTESIAN_POINT('',(3.5,3.4,1.));
#12497=CARTESIAN_POINT('Origin',(4.4,3.4,1.));
#12498=CARTESIAN_POINT('Origin',(5.,-4.,11.));
#12499=CARTESIAN_POINT('',(5.,4.,11.5));
#12500=CARTESIAN_POINT('',(5.,4.,11.));
#12501=CARTESIAN_POINT('',(5.,-4.,11.5));
#12502=CARTESIAN_POINT('',(5.,-4.,11.5));
#12503=CARTESIAN_POINT('',(5.,-4.,1.5));
#12504=CARTESIAN_POINT('',(5.,-4.,11.));
#12505=CARTESIAN_POINT('',(5.,-2.8,1.5));
#12506=CARTESIAN_POINT('',(5.,-3.7,1.5));
#12507=CARTESIAN_POINT('',(5.,-2.8,11.));
#12508=CARTESIAN_POINT('',(5.,-2.8,1.));
#12509=CARTESIAN_POINT('',(5.,2.8,11.));
#12510=CARTESIAN_POINT('',(5.,-4.,11.));
#12511=CARTESIAN_POINT('',(5.,2.8,1.));
#12512=CARTESIAN_POINT('Origin',(5.,4.,11.));
#12513=CARTESIAN_POINT('',(3.8,4.,11.));
#12514=CARTESIAN_POINT('',(3.8,4.,11.2));
#12515=CARTESIAN_POINT('',(-3.8,4.,11.));
#12516=CARTESIAN_POINT('',(5.,4.,11.));
#12517=CARTESIAN_POINT('',(-3.8,4.,1.5));
#12518=CARTESIAN_POINT('',(-3.8,4.,1.));
#12519=CARTESIAN_POINT('',(-5.,4.,1.5));
#12520=CARTESIAN_POINT('',(0.3,4.,1.5));
#12521=CARTESIAN_POINT('',(-5.,4.,11.5));
#12522=CARTESIAN_POINT('',(-5.,4.,11.));
#12523=CARTESIAN_POINT('',(5.,4.,11.5));
#12524=CARTESIAN_POINT('Origin',(4.4,-3.4,1.5));
#12525=CARTESIAN_POINT('',(4.,-3.4,1.5));
#12526=CARTESIAN_POINT('Origin',(4.4,-3.4,1.5));
#12527=CARTESIAN_POINT('',(4.,-3.4,11.5));
#12528=CARTESIAN_POINT('',(4.,-3.4,1.5));
#12529=CARTESIAN_POINT('Origin',(4.4,-3.4,11.5));
#12530=CARTESIAN_POINT('Origin',(4.4,-3.4,1.5));
#12531=CARTESIAN_POINT('',(4.175,-3.4,1.5));
#12532=CARTESIAN_POINT('Origin',(4.4,-3.4,1.5));
#12533=CARTESIAN_POINT('Origin',(4.4,-3.4,0.9));
#12534=CARTESIAN_POINT('',(4.175,-3.4,1.));
#12535=CARTESIAN_POINT('Origin',(4.4,-3.4,1.));
#12536=CARTESIAN_POINT('',(4.175,-3.4,0.9));
#12537=CARTESIAN_POINT('Origin',(4.4,-3.4,1.5));
#12538=CARTESIAN_POINT('',(3.5,-3.4,1.5));
#12539=CARTESIAN_POINT('Origin',(4.4,-3.4,1.5));
#12540=CARTESIAN_POINT('',(3.8,-4.,1.5));
#12541=CARTESIAN_POINT('',(-0.3,-4.,1.5));
#12542=CARTESIAN_POINT('',(3.8,-2.8,1.5));
#12543=CARTESIAN_POINT('',(3.8,-3.7,1.5));
#12544=CARTESIAN_POINT('',(4.4,-2.8,1.5));
#12545=CARTESIAN_POINT('Origin',(4.4,-3.4,1.));
#12546=CARTESIAN_POINT('',(3.5,-3.4,1.));
#12547=CARTESIAN_POINT('',(3.5,-3.4,1.));
#12548=CARTESIAN_POINT('Origin',(4.4,-3.4,1.));
#12549=CARTESIAN_POINT('Origin',(4.4,-2.8,6.1));
#12550=CARTESIAN_POINT('',(3.8,-2.8,11.));
#12551=CARTESIAN_POINT('',(3.8,-2.8,11.2));
#12552=CARTESIAN_POINT('',(2.2,-2.8,11.));
#12553=CARTESIAN_POINT('Origin',(3.8,-4.,1.));
#12554=CARTESIAN_POINT('',(3.8,-4.,11.));
#12555=CARTESIAN_POINT('',(3.8,-4.,11.2));
#12556=CARTESIAN_POINT('',(3.8,-2.,11.));
#12557=CARTESIAN_POINT('Origin',(-4.4,3.4,1.5));
#12558=CARTESIAN_POINT('',(-4.8,3.4,1.5));
#12559=CARTESIAN_POINT('Origin',(-4.4,3.4,1.5));
#12560=CARTESIAN_POINT('',(-4.8,3.4,11.5));
#12561=CARTESIAN_POINT('',(-4.8,3.4,1.5));
#12562=CARTESIAN_POINT('Origin',(-4.4,3.4,11.5));
#12563=CARTESIAN_POINT('Origin',(-4.4,3.4,1.5));
#12564=CARTESIAN_POINT('',(-4.625,3.4,1.5));
#12565=CARTESIAN_POINT('Origin',(-4.4,3.4,1.5));
#12566=CARTESIAN_POINT('Origin',(-4.4,3.4,0.9));
#12567=CARTESIAN_POINT('',(-4.625,3.4,1.));
#12568=CARTESIAN_POINT('Origin',(-4.4,3.4,1.));
#12569=CARTESIAN_POINT('',(-4.625,3.4,0.9));
#12570=CARTESIAN_POINT('Origin',(-4.4,3.4,1.5));
#12571=CARTESIAN_POINT('',(-5.3,3.4,1.5));
#12572=CARTESIAN_POINT('Origin',(-4.4,3.4,1.5));
#12573=CARTESIAN_POINT('',(-3.8,2.8,1.5));
#12574=CARTESIAN_POINT('',(-3.8,3.1,1.5));
#12575=CARTESIAN_POINT('',(-5.,2.8,1.5));
#12576=CARTESIAN_POINT('',(-4.4,2.8,1.5));
#12577=CARTESIAN_POINT('',(-5.,3.7,1.5));
#12578=CARTESIAN_POINT('Origin',(-4.4,3.4,1.));
#12579=CARTESIAN_POINT('',(-5.3,3.4,1.));
#12580=CARTESIAN_POINT('',(-5.3,3.4,1.));
#12581=CARTESIAN_POINT('Origin',(-4.4,3.4,1.));
#12582=CARTESIAN_POINT('Origin',(-4.4,2.8,6.1));
#12583=CARTESIAN_POINT('',(-3.8,2.8,11.));
#12584=CARTESIAN_POINT('',(-3.8,2.8,1.));
#12585=CARTESIAN_POINT('',(-5.,2.8,11.));
#12586=CARTESIAN_POINT('',(-2.2,2.8,11.));
#12587=CARTESIAN_POINT('',(-5.,2.8,11.2));
#12588=CARTESIAN_POINT('Origin',(-3.8,2.8,11.2));
#12589=CARTESIAN_POINT('',(-3.8,1.4,11.));
#12590=CARTESIAN_POINT('Origin',(-4.4,-3.4,1.5));
#12591=CARTESIAN_POINT('',(-4.8,-3.4,1.5));
#12592=CARTESIAN_POINT('Origin',(-4.4,-3.4,1.5));
#12593=CARTESIAN_POINT('',(-4.8,-3.4,11.5));
#12594=CARTESIAN_POINT('',(-4.8,-3.4,1.5));
#12595=CARTESIAN_POINT('Origin',(-4.4,-3.4,11.5));
#12596=CARTESIAN_POINT('Origin',(-4.4,-3.4,1.5));
#12597=CARTESIAN_POINT('',(-4.625,-3.4,1.5));
#12598=CARTESIAN_POINT('Origin',(-4.4,-3.4,1.5));
#12599=CARTESIAN_POINT('Origin',(-4.4,-3.4,0.9));
#12600=CARTESIAN_POINT('',(-4.625,-3.4,1.));
#12601=CARTESIAN_POINT('Origin',(-4.4,-3.4,1.));
#12602=CARTESIAN_POINT('',(-4.625,-3.4,0.9));
#12603=CARTESIAN_POINT('Origin',(-4.4,-3.4,1.5));
#12604=CARTESIAN_POINT('',(-5.3,-3.4,1.5));
#12605=CARTESIAN_POINT('Origin',(-4.4,-3.4,1.5));
#12606=CARTESIAN_POINT('',(-3.8,-2.8,1.5));
#12607=CARTESIAN_POINT('',(-5.,-2.8,1.5));
#12608=CARTESIAN_POINT('',(-4.4,-2.8,1.5));
#12609=CARTESIAN_POINT('',(-3.8,-4.,1.5));
#12610=CARTESIAN_POINT('',(-3.8,-3.7,1.5));
#12611=CARTESIAN_POINT('',(-5.,-4.,1.5));
#12612=CARTESIAN_POINT('',(-4.7,-4.,1.5));
#12613=CARTESIAN_POINT('',(-5.,0.3,1.5));
#12614=CARTESIAN_POINT('Origin',(-4.4,-3.4,1.));
#12615=CARTESIAN_POINT('',(-5.3,-3.4,1.));
#12616=CARTESIAN_POINT('',(-5.3,-3.4,1.));
#12617=CARTESIAN_POINT('Origin',(-4.4,-3.4,1.));
#12618=CARTESIAN_POINT('Origin',(-5.,-4.,11.));
#12619=CARTESIAN_POINT('',(-5.,-4.,11.5));
#12620=CARTESIAN_POINT('',(-5.,-4.,11.5));
#12621=CARTESIAN_POINT('',(-5.,-4.,11.));
#12622=CARTESIAN_POINT('',(-3.8,-4.,11.));
#12623=CARTESIAN_POINT('',(-3.8,-4.,1.));
#12624=CARTESIAN_POINT('',(-5.,-4.,11.));
#12625=CARTESIAN_POINT('Origin',(-3.8,-4.,11.2));
#12626=CARTESIAN_POINT('',(-3.8,-2.8,11.));
#12627=CARTESIAN_POINT('',(-3.8,-2.8,1.));
#12628=CARTESIAN_POINT('',(-3.8,-2.,11.));
#12629=CARTESIAN_POINT('Origin',(-3.,-2.,10.9));
#12630=CARTESIAN_POINT('',(-3.,-2.,11.));
#12631=CARTESIAN_POINT('',(3.,-2.,11.));
#12632=CARTESIAN_POINT('',(-1.5,-2.,11.));
#12633=CARTESIAN_POINT('',(-3.,-2.,11.5));
#12634=CARTESIAN_POINT('',(-3.,-2.,10.9));
#12635=CARTESIAN_POINT('',(3.,-2.,11.5));
#12636=CARTESIAN_POINT('',(-1.5,-2.,11.5));
#12637=CARTESIAN_POINT('',(3.,-2.,10.9));
#12638=CARTESIAN_POINT('Origin',(3.,-2.,10.9));
#12639=CARTESIAN_POINT('',(3.,2.,11.));
#12640=CARTESIAN_POINT('',(3.,-1.,11.));
#12641=CARTESIAN_POINT('',(3.,2.,11.5));
#12642=CARTESIAN_POINT('',(3.,-1.,11.5));
#12643=CARTESIAN_POINT('',(3.,2.,10.9));
#12644=CARTESIAN_POINT('Origin',(3.,2.,10.9));
#12645=CARTESIAN_POINT('',(-3.,2.,11.));
#12646=CARTESIAN_POINT('',(1.5,2.,11.));
#12647=CARTESIAN_POINT('',(-3.,2.,11.5));
#12648=CARTESIAN_POINT('',(1.5,2.,11.5));
#12649=CARTESIAN_POINT('',(-3.,2.,10.9));
#12650=CARTESIAN_POINT('Origin',(-3.,2.,10.9));
#12651=CARTESIAN_POINT('',(-3.,1.,11.));
#12652=CARTESIAN_POINT('',(-3.,1.,11.5));
#12653=CARTESIAN_POINT('Origin',(3.8,2.8,1.));
#12654=CARTESIAN_POINT('',(3.8,2.8,11.));
#12655=CARTESIAN_POINT('',(3.8,2.8,11.2));
#12656=CARTESIAN_POINT('',(3.8,1.4,11.));
#12657=CARTESIAN_POINT('Origin',(5.,2.8,1.));
#12658=CARTESIAN_POINT('Origin',(4.4,2.8,6.1));
#12659=CARTESIAN_POINT('',(2.2,2.8,11.));
#12660=CARTESIAN_POINT('Origin',(0.,0.,11.));
#12661=CARTESIAN_POINT('',(-5.,-2.8,11.));
#12662=CARTESIAN_POINT('',(-2.2,-2.8,11.));
#12663=CARTESIAN_POINT('',(-5.,4.,11.));
#12664=CARTESIAN_POINT('Origin',(5.,-4.,1.));
#12665=CARTESIAN_POINT('Origin',(-3.8,2.8,1.));
#12666=CARTESIAN_POINT('Origin',(-4.4,-2.8,6.1));
#12667=CARTESIAN_POINT('',(-5.,-2.8,11.2));
#12668=CARTESIAN_POINT('Origin',(-3.8,-4.,1.));
#12669=CARTESIAN_POINT('Origin',(-5.,4.,11.));
#12670=CARTESIAN_POINT('',(-5.,4.,11.5));
#12671=CARTESIAN_POINT('Origin',(0.,0.,11.5));
#12672=CARTESIAN_POINT('',(0.,0.,0.));
#12673=CARTESIAN_POINT('Origin',(-4.5,11.,-0.5));
#12674=CARTESIAN_POINT('',(-4.5,11.,-0.5));
#12675=CARTESIAN_POINT('',(-6.5,11.,-0.5));
#12676=CARTESIAN_POINT('',(-4.5,11.,-0.5));
#12677=CARTESIAN_POINT('',(-6.5,11.,0.));
#12678=CARTESIAN_POINT('',(-6.5,11.,-0.5));
#12679=CARTESIAN_POINT('',(-4.5,11.,0.));
#12680=CARTESIAN_POINT('',(-4.5,11.,0.));
#12681=CARTESIAN_POINT('',(-4.5,11.,-0.5));
#12682=CARTESIAN_POINT('Origin',(-4.5,-11.,-0.5));
#12683=CARTESIAN_POINT('',(-4.5,-11.,-0.5));
#12684=CARTESIAN_POINT('',(-4.5,-11.,-0.5));
#12685=CARTESIAN_POINT('',(-4.5,-11.,0.));
#12686=CARTESIAN_POINT('',(-4.5,-11.,0.));
#12687=CARTESIAN_POINT('',(-4.5,-11.,-0.5));
#12688=CARTESIAN_POINT('Origin',(-6.5,-11.,-0.5));
#12689=CARTESIAN_POINT('',(-6.5,-11.,-0.5));
#12690=CARTESIAN_POINT('',(-6.5,-11.,-0.5));
#12691=CARTESIAN_POINT('',(-6.5,-11.,0.));
#12692=CARTESIAN_POINT('',(-6.5,-11.,0.));
#12693=CARTESIAN_POINT('',(-6.5,-11.,-0.5));
#12694=CARTESIAN_POINT('Origin',(-6.5,11.,-0.5));
#12695=CARTESIAN_POINT('',(-6.5,11.,-0.5));
#12696=CARTESIAN_POINT('',(-6.5,11.,0.));
#12697=CARTESIAN_POINT('Origin',(-5.5,0.,0.));
#12698=CARTESIAN_POINT('Origin',(-5.5,0.,-0.5));
#12699=CARTESIAN_POINT('',(0.,0.,0.));
#12700=CARTESIAN_POINT('Origin',(12.5,11.,-0.5));
#12701=CARTESIAN_POINT('',(12.5,11.,-0.5));
#12702=CARTESIAN_POINT('',(10.5,11.,-0.5));
#12703=CARTESIAN_POINT('',(12.5,11.,-0.5));
#12704=CARTESIAN_POINT('',(10.5,11.,0.));
#12705=CARTESIAN_POINT('',(10.5,11.,-0.5));
#12706=CARTESIAN_POINT('',(12.5,11.,0.));
#12707=CARTESIAN_POINT('',(12.5,11.,0.));
#12708=CARTESIAN_POINT('',(12.5,11.,-0.5));
#12709=CARTESIAN_POINT('Origin',(12.5,-11.,-0.5));
#12710=CARTESIAN_POINT('',(12.5,-11.,-0.5));
#12711=CARTESIAN_POINT('',(12.5,-11.,-0.5));
#12712=CARTESIAN_POINT('',(12.5,-11.,0.));
#12713=CARTESIAN_POINT('',(12.5,-11.,0.));
#12714=CARTESIAN_POINT('',(12.5,-11.,-0.5));
#12715=CARTESIAN_POINT('Origin',(10.5,-11.,-0.5));
#12716=CARTESIAN_POINT('',(10.5,-11.,-0.5));
#12717=CARTESIAN_POINT('',(10.5,-11.,-0.5));
#12718=CARTESIAN_POINT('',(10.5,-11.,0.));
#12719=CARTESIAN_POINT('',(10.5,-11.,0.));
#12720=CARTESIAN_POINT('',(10.5,-11.,-0.5));
#12721=CARTESIAN_POINT('Origin',(10.5,11.,-0.5));
#12722=CARTESIAN_POINT('',(10.5,11.,-0.5));
#12723=CARTESIAN_POINT('',(10.5,11.,0.));
#12724=CARTESIAN_POINT('Origin',(11.5,0.,0.));
#12725=CARTESIAN_POINT('Origin',(11.5,0.,-0.5));
#12726=CARTESIAN_POINT('',(0.,0.,0.));
#12727=CARTESIAN_POINT('Origin',(0.144337567297406,-0.6,-0.25));
#12728=CARTESIAN_POINT('',(0.288675134594813,-0.6,0.));
#12729=CARTESIAN_POINT('',(0.144337567297406,-0.6,-0.25));
#12730=CARTESIAN_POINT('',(0.288675134594813,-0.6,0.));
#12731=CARTESIAN_POINT('',(0.144337567297406,-0.96,-0.25));
#12732=CARTESIAN_POINT('',(0.144337567297406,-0.6,-0.25));
#12733=CARTESIAN_POINT('',(0.288675134594813,-0.96,0.));
#12734=CARTESIAN_POINT('',(0.288675134594813,-0.96,0.));
#12735=CARTESIAN_POINT('',(0.288675134594813,-0.6,0.));
#12736=CARTESIAN_POINT('Origin',(-0.144337567297406,-0.6,-0.25));
#12737=CARTESIAN_POINT('',(-0.144337567297406,-0.6,-0.25));
#12738=CARTESIAN_POINT('',(0.144337567297406,-0.6,-0.25));
#12739=CARTESIAN_POINT('',(-0.144337567297406,-0.96,-0.25));
#12740=CARTESIAN_POINT('',(-0.144337567297406,-0.6,-0.25));
#12741=CARTESIAN_POINT('',(0.144337567297406,-0.96,-0.25));
#12742=CARTESIAN_POINT('Origin',(-0.288675134594813,-0.6,-8.32667268468867E-17));
#12743=CARTESIAN_POINT('',(-0.288675134594813,-0.6,-3.53525079574969E-17));
#12744=CARTESIAN_POINT('',(-0.144337567297406,-0.6,-0.25));
#12745=CARTESIAN_POINT('',(-0.288675134594813,-0.96,-5.55111512312578E-17));
#12746=CARTESIAN_POINT('',(-0.288675134594813,-0.6,-3.53525079574969E-17));
#12747=CARTESIAN_POINT('',(-0.144337567297406,-0.96,-0.25));
#12748=CARTESIAN_POINT('Origin',(-0.144337567297407,-0.6,0.25));
#12749=CARTESIAN_POINT('',(-0.144337567297407,-0.6,0.25));
#12750=CARTESIAN_POINT('',(-0.288675134594813,-0.6,-3.53525079574969E-17));
#12751=CARTESIAN_POINT('',(-0.144337567297407,-0.96,0.25));
#12752=CARTESIAN_POINT('',(-0.144337567297407,-0.6,0.25));
#12753=CARTESIAN_POINT('',(-0.288675134594813,-0.96,-3.53525079574969E-17));
#12754=CARTESIAN_POINT('Origin',(0.144337567297406,-0.6,0.25));
#12755=CARTESIAN_POINT('',(0.144337567297406,-0.6,0.25));
#12756=CARTESIAN_POINT('',(-0.144337567297407,-0.6,0.25));
#12757=CARTESIAN_POINT('',(0.144337567297406,-0.96,0.25));
#12758=CARTESIAN_POINT('',(0.144337567297406,-0.6,0.25));
#12759=CARTESIAN_POINT('',(-0.144337567297407,-0.96,0.25));
#12760=CARTESIAN_POINT('Origin',(0.288675134594813,-0.6,0.));
#12761=CARTESIAN_POINT('',(0.144337567297406,-0.6,0.25));
#12762=CARTESIAN_POINT('',(0.144337567297406,-0.96,0.25));
#12763=CARTESIAN_POINT('Origin',(0.,-0.6,0.));
#12764=CARTESIAN_POINT('Origin',(0.,-0.96,0.));
#12765=CARTESIAN_POINT('Origin',(0.,-1.8,0.));
#12766=CARTESIAN_POINT('',(-0.2942,-1.8,3.60291088309151E-17));
#12767=CARTESIAN_POINT('Origin',(0.,-1.8,0.));
#12768=CARTESIAN_POINT('Origin',(0.45,0.6,0.));
#12769=CARTESIAN_POINT('',(-0.45,0.6,-5.51091059616309E-17));
#12770=CARTESIAN_POINT('Origin',(0.,0.6,0.));
#12771=CARTESIAN_POINT('Origin',(0.,0.575,0.));
#12772=CARTESIAN_POINT('',(-0.5,0.55,-6.12323399573677E-17));
#12773=CARTESIAN_POINT('Origin',(0.,0.55,0.));
#12774=CARTESIAN_POINT('',(-0.475,0.575,-5.81707229594993E-17));
#12775=CARTESIAN_POINT('Origin',(0.,0.29,0.));
#12776=CARTESIAN_POINT('',(-0.5,0.0299999999999998,-6.12323399573677E-17));
#12777=CARTESIAN_POINT('Origin',(0.,0.0299999999999998,0.));
#12778=CARTESIAN_POINT('',(-0.5,0.29,-6.12323399573677E-17));
#12779=CARTESIAN_POINT('Origin',(0.,0.0150000000000001,0.));
#12780=CARTESIAN_POINT('',(-0.47,7.11236625150491E-17,-5.75583995599256E-17));
#12781=CARTESIAN_POINT('Origin',(0.,0.,0.));
#12782=CARTESIAN_POINT('',(-0.485,0.0150000000000001,-5.93953697586466E-17));
#12783=CARTESIAN_POINT('Origin',(0.32,0.,0.));
#12784=CARTESIAN_POINT('',(-0.32,-6.93889390390723E-18,-3.91886975727153E-17));
#12785=CARTESIAN_POINT('Origin',(0.,0.,0.));
#12786=CARTESIAN_POINT('Origin',(0.,-0.02,0.));
#12787=CARTESIAN_POINT('',(-0.2942,-0.0515999999999999,3.60291088309151E-17));
#12788=CARTESIAN_POINT('Origin',(0.,-0.0515999999999999,0.));
#12789=CARTESIAN_POINT('',(-0.31,-0.02,-3.7964050773568E-17));
#12790=CARTESIAN_POINT('Origin',(0.,-1.24,0.));
#12791=CARTESIAN_POINT('',(-0.2942,-1.24,-3.60291088309151E-17));
#12792=CARTESIAN_POINT('',(0.,0.,0.));
#12793=CARTESIAN_POINT('',(0.,0.,0.));
#12794=CARTESIAN_POINT('Origin',(0.,0.,0.));
#12795=CARTESIAN_POINT('',(-1.070235,-0.308121667383195,-1.31065986708547E-16));
#12796=CARTESIAN_POINT('',(-1.31065986708547E-16,-0.308121667383195,1.070235));
#12797=CARTESIAN_POINT('Origin',(0.,-0.308121667383195,0.));
#12798=CARTESIAN_POINT('Origin',(0.,-0.308121667383195,0.));
#12799=CARTESIAN_POINT('',(-1.31065986708547E-16,0.308121667383195,1.070235));
#12800=CARTESIAN_POINT('Origin',(-1.34711147906209E-16,0.,1.1));
#12801=CARTESIAN_POINT('',(-1.070235,0.308121667383195,1.31065986708547E-16));
#12802=CARTESIAN_POINT('Origin',(0.,0.308121667383195,0.));
#12803=CARTESIAN_POINT('Origin',(0.,0.308121667383195,0.));
#12804=CARTESIAN_POINT('Origin',(0.,0.,0.));
#12805=CARTESIAN_POINT('',(-1.070235,0.5,-1.31065986708547E-16));
#12806=CARTESIAN_POINT('',(-1.070235,0.,-1.31065986708547E-16));
#12807=CARTESIAN_POINT('Origin',(0.,0.5,0.));
#12808=CARTESIAN_POINT('Origin',(0.,0.,0.));
#12809=CARTESIAN_POINT('',(-0.6,-0.44,-7.34788079488412E-17));
#12810=CARTESIAN_POINT('Origin',(0.,-0.44,0.));
#12811=CARTESIAN_POINT('',(-0.6,0.44,-7.34788079488412E-17));
#12812=CARTESIAN_POINT('',(-0.6,0.,-7.34788079488412E-17));
#12813=CARTESIAN_POINT('Origin',(0.,0.44,0.));
#12814=CARTESIAN_POINT('Origin',(0.,0.47,0.));
#12815=CARTESIAN_POINT('',(-0.66,0.5,-8.08266887437253E-17));
#12816=CARTESIAN_POINT('',(-0.63,0.47,-7.71527483462832E-17));
#12817=CARTESIAN_POINT('Origin',(0.,0.5,0.));
#12818=CARTESIAN_POINT('Origin',(1.070235,0.5,0.));
#12819=CARTESIAN_POINT('Origin',(0.,0.,0.));
#12820=CARTESIAN_POINT('',(-1.070235,-0.5,-1.31065986708547E-16));
#12821=CARTESIAN_POINT('Origin',(0.,-0.5,0.));
#12822=CARTESIAN_POINT('',(-1.070235,0.,-1.31065986708547E-16));
#12823=CARTESIAN_POINT('Origin',(0.66,-0.5,0.));
#12824=CARTESIAN_POINT('',(-0.66,-0.5,-8.08266887437253E-17));
#12825=CARTESIAN_POINT('Origin',(0.,-0.5,0.));
#12826=CARTESIAN_POINT('Origin',(0.,-0.47,0.));
#12827=CARTESIAN_POINT('',(-0.63,-0.47,-7.71527483462832E-17));
#12828=CARTESIAN_POINT('',(0.,0.,0.));
#12829=CARTESIAN_POINT('Origin',(0.,0.,0.));
#12830=CARTESIAN_POINT('',(-1.129765,0.308121667383195,-1.38356309103871E-16));
#12831=CARTESIAN_POINT('',(-1.38356309103871E-16,0.308121667383195,1.129765));
#12832=CARTESIAN_POINT('Origin',(0.,0.308121667383195,0.));
#12833=CARTESIAN_POINT('Origin',(0.,0.308121667383195,0.));
#12834=CARTESIAN_POINT('',(-1.38356309103871E-16,-0.308121667383195,1.129765));
#12835=CARTESIAN_POINT('Origin',(-1.34711147906209E-16,0.,1.1));
#12836=CARTESIAN_POINT('',(-1.129765,-0.308121667383195,1.38356309103871E-16));
#12837=CARTESIAN_POINT('Origin',(0.,-0.308121667383195,0.));
#12838=CARTESIAN_POINT('Origin',(0.,-0.308121667383195,0.));
#12839=CARTESIAN_POINT('Origin',(0.,0.,0.));
#12840=CARTESIAN_POINT('',(-1.129765,-0.5,-1.38356309103871E-16));
#12841=CARTESIAN_POINT('Origin',(0.,-0.5,0.));
#12842=CARTESIAN_POINT('',(-1.129765,0.,-1.38356309103871E-16));
#12843=CARTESIAN_POINT('Origin',(1.54,0.5,0.));
#12844=CARTESIAN_POINT('',(-1.54,0.5,-1.88595607068692E-16));
#12845=CARTESIAN_POINT('Origin',(0.,0.5,0.));
#12846=CARTESIAN_POINT('',(-1.129765,0.5,-1.38356309103871E-16));
#12847=CARTESIAN_POINT('Origin',(0.,0.5,0.));
#12848=CARTESIAN_POINT('Origin',(0.,0.47,0.));
#12849=CARTESIAN_POINT('',(-1.6,0.44,-1.95943487863577E-16));
#12850=CARTESIAN_POINT('Origin',(0.,0.44,0.));
#12851=CARTESIAN_POINT('',(-1.57,0.47,-1.92269547466134E-16));
#12852=CARTESIAN_POINT('Origin',(0.,0.,0.));
#12853=CARTESIAN_POINT('',(-1.6,-0.44,-1.95943487863577E-16));
#12854=CARTESIAN_POINT('Origin',(0.,-0.44,0.));
#12855=CARTESIAN_POINT('',(-1.6,0.,-1.95943487863577E-16));
#12856=CARTESIAN_POINT('Origin',(0.,-0.47,0.));
#12857=CARTESIAN_POINT('',(-1.54,-0.5,-1.88595607068692E-16));
#12858=CARTESIAN_POINT('Origin',(0.,-0.5,0.));
#12859=CARTESIAN_POINT('',(-1.57,-0.47,-1.92269547466134E-16));
#12860=CARTESIAN_POINT('Origin',(1.129765,-0.5,0.));
#12861=CARTESIAN_POINT('Origin',(0.,0.,0.));
#12862=CARTESIAN_POINT('',(-1.129765,0.,-1.38356309103871E-16));
#12863=CARTESIAN_POINT('',(0.,0.,0.));
#12864=CARTESIAN_POINT('Origin',(1.1,0.,0.));
#12865=CARTESIAN_POINT('',(1.1,-2.23201749654651E-33,0.29765));
#12866=CARTESIAN_POINT('',(1.1,-2.23201749654651E-33,-0.29765));
#12867=CARTESIAN_POINT('Origin',(1.1,0.,0.));
#12868=CARTESIAN_POINT('Origin',(0.685838782044607,0.,-0.860014630714833));
#12869=CARTESIAN_POINT('',(0.918550922801216,-5.31350540756609E-33,-0.674432891191581));
#12870=CARTESIAN_POINT('',(0.453126641287998,8.49470414473068E-34,-1.04559637023808));
#12871=CARTESIAN_POINT('Origin',(0.685838782044607,0.,-0.860014630714833));
#12872=CARTESIAN_POINT('Origin',(-0.244773027351946,0.,-1.07242070340001));
#12873=CARTESIAN_POINT('',(0.0454142657089739,-2.23201749654651E-33,-1.1386540593921));
#12874=CARTESIAN_POINT('',(-0.534960320412865,-2.23201749654651E-33,-1.00618734740791));
#12875=CARTESIAN_POINT('Origin',(-0.244773027351946,0.,-1.07242070340001));
#12876=CARTESIAN_POINT('Origin',(-0.991065754692661,0.,-0.477272113029314));
#12877=CARTESIAN_POINT('',(-0.86192025974432,8.49470414473067E-34,-0.745445496560469));
#12878=CARTESIAN_POINT('',(-1.120211249641,-5.31350540756609E-33,-0.209098729498159));
#12879=CARTESIAN_POINT('Origin',(-0.991065754692661,0.,-0.477272113029314));
#12880=CARTESIAN_POINT('Origin',(-0.991065754692661,0.,0.477272113029314));
#12881=CARTESIAN_POINT('',(-1.120211249641,-2.23201749654651E-33,0.209098729498159));
#12882=CARTESIAN_POINT('',(-0.86192025974432,-2.23201749654651E-33,0.745445496560469));
#12883=CARTESIAN_POINT('Origin',(-0.991065754692661,0.,0.477272113029314));
#12884=CARTESIAN_POINT('Origin',(-0.244773027351946,0.,1.07242070340001));
#12885=CARTESIAN_POINT('',(-0.534960320412866,-2.23201749654651E-33,1.00618734740791));
#12886=CARTESIAN_POINT('',(0.0454142657089737,-2.23201749654651E-33,1.1386540593921));
#12887=CARTESIAN_POINT('Origin',(-0.244773027351946,0.,1.07242070340001));
#12888=CARTESIAN_POINT('Origin',(0.685838782044607,0.,0.860014630714833));
#12889=CARTESIAN_POINT('',(0.453126641287998,-2.23201749654651E-33,1.04559637023808));
#12890=CARTESIAN_POINT('',(0.918550922801216,-2.23201749654651E-33,0.674432891191581));
#12891=CARTESIAN_POINT('Origin',(0.685838782044607,0.,0.860014630714833));
#12892=CARTESIAN_POINT('',(0.,0.,0.));
#12893=CARTESIAN_POINT('Origin',(0.685838782044607,0.,0.860014630714833));
#12894=CARTESIAN_POINT('',(0.413083465285518,-0.05953,0.993751811093549));
#12895=CARTESIAN_POINT('',(0.876916659919095,-0.05953,0.623857181492959));
#12896=CARTESIAN_POINT('Ctrl Pts',(0.413083465285518,-0.05953,0.993751811093549));
#12897=CARTESIAN_POINT('Ctrl Pts',(0.419070565453383,-0.0925528133349865,
0.991263089003441));
#12898=CARTESIAN_POINT('Ctrl Pts',(0.430199341854858,-0.124911173756694,
0.986608710139579));
#12899=CARTESIAN_POINT('Ctrl Pts',(0.457978755888596,-0.177924977804098,
0.973971221090534));
#12900=CARTESIAN_POINT('Ctrl Pts',(0.473077587363685,-0.199697230012983,
0.966820759530997));
#12901=CARTESIAN_POINT('Ctrl Pts',(0.507057380724533,-0.237895043532788,
0.949440676105255));
#12902=CARTESIAN_POINT('Ctrl Pts',(0.525933334162555,-0.254319232363049,
0.939198248544428));
#12903=CARTESIAN_POINT('Ctrl Pts',(0.564362943424238,-0.28018331644634,
0.916597376014514));
#12904=CARTESIAN_POINT('Ctrl Pts',(0.585840553788742,-0.29104845371857,
0.903141581680914));
#12905=CARTESIAN_POINT('Ctrl Pts',(0.629305439856167,-0.30527573347708,
0.873412008702649));
#12906=CARTESIAN_POINT('Ctrl Pts',(0.651278921914856,-0.308638795020976,
0.857118508332695));
#12907=CARTESIAN_POINT('Ctrl Pts',(0.690705563850638,-0.308638795020976,
0.825676810575914));
#12908=CARTESIAN_POINT('Ctrl Pts',(0.711480111898423,-0.30527573347708,
0.807879894508811));
#12909=CARTESIAN_POINT('Ctrl Pts',(0.750136149454208,-0.29104845371857,
0.772120216227122));
#12910=CARTESIAN_POINT('Ctrl Pts',(0.768033796848072,-0.28018331644634,
0.754175290318038));
#12911=CARTESIAN_POINT('Ctrl Pts',(0.798619410861634,-0.254319232363049,
0.721738358858166));
#12912=CARTESIAN_POINT('Ctrl Pts',(0.812805334167529,-0.237895043532788,
0.705614819529209));
#12913=CARTESIAN_POINT('Ctrl Pts',(0.837310877969633,-0.199697230012983,
0.676354402927683));
#12914=CARTESIAN_POINT('Ctrl Pts',(0.847641868610495,-0.177924977804098,
0.663225258065736));
#12915=CARTESIAN_POINT('Ctrl Pts',(0.866144010579847,-0.124911173756694,
0.638954437806245));
#12916=CARTESIAN_POINT('Ctrl Pts',(0.873158080166742,-0.0925528133349865,
0.62914037979579));
#12917=CARTESIAN_POINT('Ctrl Pts',(0.876916659919095,-0.05953,0.623857181492959));
#12918=CARTESIAN_POINT('',(0.437601487681057,-0.05953,1.03511272300331));
#12919=CARTESIAN_POINT('Origin',(0.685838782044607,-0.05953,0.860014630714833));
#12920=CARTESIAN_POINT('',(0.911784794170997,-0.05953,0.656964154625313));
#12921=CARTESIAN_POINT('Ctrl Pts',(0.911784794170998,-0.0595300000000001,
0.656964154625312));
#12922=CARTESIAN_POINT('Ctrl Pts',(0.909827729890942,-0.0762225747374255,
0.659680317203144));
#12923=CARTESIAN_POINT('Ctrl Pts',(0.907004864562642,-0.0928409665394228,
0.663576540841106));
#12924=CARTESIAN_POINT('Ctrl Pts',(0.895234408667242,-0.144299303100741,
0.679480524217551));
#12925=CARTESIAN_POINT('Ctrl Pts',(0.882797231409153,-0.177024326825049,
0.695831250979106));
#12926=CARTESIAN_POINT('Ctrl Pts',(0.854332839576145,-0.227269801620064,
0.73042219438957));
#12927=CARTESIAN_POINT('Ctrl Pts',(0.834863020612702,-0.251265615809407,
0.752807465209441));
#12928=CARTESIAN_POINT('Ctrl Pts',(0.800439809856111,-0.279889827963178,
0.789147407129766));
#12929=CARTESIAN_POINT('Ctrl Pts',(0.781998747691871,-0.290879136862659,
0.80756613568454));
#12930=CARTESIAN_POINT('Ctrl Pts',(0.742239891936898,-0.305251990234487,
0.844254137480382));
#12931=CARTESIAN_POINT('Ctrl Pts',(0.720906778729541,-0.308638795020976,
0.862505527716294));
#12932=CARTESIAN_POINT('Ctrl Pts',(0.680463863683392,-0.308638795020976,
0.894757676234429));
#12933=CARTESIAN_POINT('Ctrl Pts',(0.657923009631182,-0.305251990234488,
0.91149460735272));
#12934=CARTESIAN_POINT('Ctrl Pts',(0.613307674922609,-0.290879136862659,
0.942092777160053));
#12935=CARTESIAN_POINT('Ctrl Pts',(0.591247219971725,-0.279889827963178,
0.955972930713954));
#12936=CARTESIAN_POINT('Ctrl Pts',(0.548158511259202,-0.251265615809407,
0.981446681891443));
#12937=CARTESIAN_POINT('Ctrl Pts',(0.522002043615455,-0.227269801620063,
0.995447160474328));
#12938=CARTESIAN_POINT('Ctrl Pts',(0.481944444320713,-0.177024326825049,
1.01550068154148));
#12939=CARTESIAN_POINT('Ctrl Pts',(0.463236132117164,-0.14429930310074,
1.0239876538093));
#12940=CARTESIAN_POINT('Ctrl Pts',(0.445111721969657,-0.0928409665394226,
1.03192403056628));
#12941=CARTESIAN_POINT('Ctrl Pts',(0.440685038163619,-0.0762225747374254,
1.03380912944435));
#12942=CARTESIAN_POINT('Ctrl Pts',(0.437601487681056,-0.05953,1.03511272300331));
#12943=CARTESIAN_POINT('Origin',(0.685838782044607,-0.05953,0.860014630714833));
#12944=CARTESIAN_POINT('Origin',(0.,-0.208355,0.));
#12945=CARTESIAN_POINT('',(0.0548532617164168,-0.05953,1.12247250791415));
#12946=CARTESIAN_POINT('Origin',(0.,-0.05953,0.));
#12947=CARTESIAN_POINT('',(-0.536443649899848,-0.05953,0.987512846410683));
#12948=CARTESIAN_POINT('Ctrl Pts',(0.0548532617164173,-0.0595300000000001,
1.12247250791414));
#12949=CARTESIAN_POINT('Ctrl Pts',(0.05150947068137,-0.0762225747374254,
1.12263591311425));
#12950=CARTESIAN_POINT('Ctrl Pts',(0.0467032526342597,-0.0928409665394227,
1.12285816383385));
#12951=CARTESIAN_POINT('Ctrl Pts',(0.0269302585198975,-0.144299303100741,
1.12357162229597));
#12952=CARTESIAN_POINT('Ctrl Pts',(0.006392292392153,-0.177024326825049,
1.12404235695137));
#12953=CARTESIAN_POINT('Ctrl Pts',(-0.0383992541984087,-0.227269801620063,
1.12335509974011));
#12954=CARTESIAN_POINT('Ctrl Pts',(-0.0680399972366993,-0.251265615809407,
1.12208997038458));
#12955=CARTESIAN_POINT('Ctrl Pts',(-0.117914228755037,-0.279889827963178,
1.1178344036749));
#12956=CARTESIAN_POINT('Ctrl Pts',(-0.14381238480104,-0.290879136862659,
1.11490049012186));
#12957=CARTESIAN_POINT('Ctrl Pts',(-0.19728546073067,-0.305251990234488,
1.10669035995599));
#12958=CARTESIAN_POINT('Ctrl Pts',(-0.224855950742601,-0.308638795020976,
1.10139101611326));
#12959=CARTESIAN_POINT('Ctrl Pts',(-0.275287440920027,-0.308638795020976,
1.0898803575765));
#12960=CARTESIAN_POINT('Ctrl Pts',(-0.302426893214945,-0.305251990234488,
1.08269251410343));
#12961=CARTESIAN_POINT('Ctrl Pts',(-0.35416671187353,-0.290879136862659,
1.06688848765783));
#12962=CARTESIAN_POINT('Ctrl Pts',(-0.3787731215897,-0.279889827963178,
1.05829506364875));
#12963=CARTESIAN_POINT('Ctrl Pts',(-0.425554672694338,-0.251265615809407,
1.04048957871266));
#12964=CARTESIAN_POINT('Ctrl Pts',(-0.452808978448581,-0.227269801620063,
1.02876878445619));
#12965=CARTESIAN_POINT('Ctrl Pts',(-0.493462957200432,-0.177024326825049,
1.0099536580922));
#12966=CARTESIAN_POINT('Ctrl Pts',(-0.511762781179148,-0.14429930310074,
1.00061845128527));
#12967=CARTESIAN_POINT('Ctrl Pts',(-0.529268075276157,-0.0928409665394226,
0.991396466802468));
#12968=CARTESIAN_POINT('Ctrl Pts',(-0.533501897135713,-0.0762225747374254,
0.989110885965947));
#12969=CARTESIAN_POINT('Ctrl Pts',(-0.536443649899848,-0.0595300000000001,
0.987512846410683));
#12970=CARTESIAN_POINT('',(-0.843383895613249,-0.05953,0.742736168477219));
#12971=CARTESIAN_POINT('Origin',(0.,-0.05953,0.));
#12972=CARTESIAN_POINT('',(-1.10653577764992,-0.05953,0.196295654879792));
#12973=CARTESIAN_POINT('Ctrl Pts',(-0.843383895613249,-0.0595300000000001,
0.742736168477219));
#12974=CARTESIAN_POINT('Ctrl Pts',(-0.84559647055299,-0.0762225747374255,
0.740223768851062));
#12975=CARTESIAN_POINT('Ctrl Pts',(-0.848766861100456,-0.0928409665394227,
0.736604687327351));
#12976=CARTESIAN_POINT('Ctrl Pts',(-0.861652925570091,-0.144299303100741,
0.721590372101268));
#12977=CARTESIAN_POINT('Ctrl Pts',(-0.87482617317514,-0.177024326825049,
0.705826641853758));
#12978=CARTESIAN_POINT('Ctrl Pts',(-0.902215926359523,-0.227269801620063,
0.670378702718353));
#12979=CARTESIAN_POINT('Ctrl Pts',(-0.919707509403859,-0.251265615809407,
0.646415841396062));
#12980=CARTESIAN_POINT('Ctrl Pts',(-0.947476448101718,-0.279889827963178,
0.604769294586516));
#12981=CARTESIAN_POINT('Ctrl Pts',(-0.961329858300736,-0.290879136862659,
0.582692035672022));
#12982=CARTESIAN_POINT('Ctrl Pts',(-0.988250837578047,-0.305251990234488,
0.535766169015486));
#12983=CARTESIAN_POINT('Ctrl Pts',(-1.00129756308006,-0.308638795020976,
0.510906605094603));
#12984=CARTESIAN_POINT('Ctrl Pts',(-1.02374168767024,-0.308638795020976,
0.46430090015576));
#12985=CARTESIAN_POINT('Ctrl Pts',(-1.03504317708586,-0.305251990234488,
0.438600874831839));
#12986=CARTESIAN_POINT('Ctrl Pts',(-1.05494634094458,-0.290879136862659,
0.388295406390235));
#12987=CARTESIAN_POINT('Ctrl Pts',(-1.06356957703048,-0.279889827963178,
0.363699428370917));
#12988=CARTESIAN_POINT('Ctrl Pts',(-1.0788165083757,-0.251265615809407,
0.316022600643821));
#12989=CARTESIAN_POINT('Ctrl Pts',(-1.08664560412098,-0.227269801620063,
0.287406530683752));
#12990=CARTESIAN_POINT('Ctrl Pts',(-1.09728268713976,-0.177024326825049,
0.243890930799337));
#12991=CARTESIAN_POINT('Ctrl Pts',(-1.10139388218929,-0.144299303100741,
0.22376314604679));
#12992=CARTESIAN_POINT('Ctrl Pts',(-1.10509821673782,-0.0928409665394227,
0.204327142733961));
#12993=CARTESIAN_POINT('Ctrl Pts',(-1.10595102243643,-0.0762225747374254,
0.199591971170104));
#12994=CARTESIAN_POINT('Ctrl Pts',(-1.10653577764992,-0.0595300000000001,
0.196295654879792));
#12995=CARTESIAN_POINT('',(-1.123812,-0.05953,1.37627276864339E-16));
#12996=CARTESIAN_POINT('Origin',(0.,-0.05953,0.));
#12997=CARTESIAN_POINT('',(-1.123812,-0.35718,1.37627276864339E-16));
#12998=CARTESIAN_POINT('',(-1.123812,-0.208355,1.37627276864339E-16));
#12999=CARTESIAN_POINT('Origin',(0.,-0.35718,0.));
#13000=CARTESIAN_POINT('',(-1.10653577764992,-0.05953,-0.196295654879793));
#13001=CARTESIAN_POINT('Origin',(0.,-0.05953,0.));
#13002=CARTESIAN_POINT('',(-0.843383895613249,-0.05953,-0.742736168477219));
#13003=CARTESIAN_POINT('Ctrl Pts',(-1.10653577764992,-0.0595300000000001,
-0.196295654879792));
#13004=CARTESIAN_POINT('Ctrl Pts',(-1.10595102243643,-0.0762225747374255,
-0.199591971170104));
#13005=CARTESIAN_POINT('Ctrl Pts',(-1.10509821673782,-0.0928409665394228,
-0.204327142733962));
#13006=CARTESIAN_POINT('Ctrl Pts',(-1.10139388218929,-0.144299303100741,
-0.22376314604679));
#13007=CARTESIAN_POINT('Ctrl Pts',(-1.09728268713976,-0.177024326825049,
-0.243890930799338));
#13008=CARTESIAN_POINT('Ctrl Pts',(-1.08664560412098,-0.227269801620063,
-0.287406530683753));
#13009=CARTESIAN_POINT('Ctrl Pts',(-1.0788165083757,-0.251265615809407,
-0.316022600643821));
#13010=CARTESIAN_POINT('Ctrl Pts',(-1.06356957703048,-0.279889827963178,
-0.363699428370918));
#13011=CARTESIAN_POINT('Ctrl Pts',(-1.05494634094458,-0.290879136862659,
-0.388295406390235));
#13012=CARTESIAN_POINT('Ctrl Pts',(-1.03504317708586,-0.305251990234488,
-0.438600874831839));
#13013=CARTESIAN_POINT('Ctrl Pts',(-1.02374168767024,-0.308638795020976,
-0.46430090015576));
#13014=CARTESIAN_POINT('Ctrl Pts',(-1.00129756308006,-0.308638795020976,
-0.510906605094603));
#13015=CARTESIAN_POINT('Ctrl Pts',(-0.988250837578047,-0.305251990234488,
-0.535766169015486));
#13016=CARTESIAN_POINT('Ctrl Pts',(-0.961329858300736,-0.290879136862659,
-0.582692035672022));
#13017=CARTESIAN_POINT('Ctrl Pts',(-0.947476448101718,-0.279889827963178,
-0.604769294586516));
#13018=CARTESIAN_POINT('Ctrl Pts',(-0.919707509403859,-0.251265615809407,
-0.646415841396062));
#13019=CARTESIAN_POINT('Ctrl Pts',(-0.902215926359523,-0.227269801620064,
-0.670378702718353));
#13020=CARTESIAN_POINT('Ctrl Pts',(-0.87482617317514,-0.177024326825049,
-0.705826641853758));
#13021=CARTESIAN_POINT('Ctrl Pts',(-0.861652925570091,-0.144299303100741,
-0.721590372101268));
#13022=CARTESIAN_POINT('Ctrl Pts',(-0.848766861100456,-0.0928409665394229,
-0.736604687327351));
#13023=CARTESIAN_POINT('Ctrl Pts',(-0.84559647055299,-0.0762225747374255,
-0.740223768851063));
#13024=CARTESIAN_POINT('Ctrl Pts',(-0.843383895613249,-0.0595300000000001,
-0.742736168477219));
#13025=CARTESIAN_POINT('',(-0.536443649899847,-0.05953,-0.987512846410683));
#13026=CARTESIAN_POINT('Origin',(0.,-0.05953,0.));
#13027=CARTESIAN_POINT('',(0.0548532617164172,-0.05953,-1.12247250791415));
#13028=CARTESIAN_POINT('Ctrl Pts',(-0.536443649899848,-0.0595300000000001,
-0.987512846410683));
#13029=CARTESIAN_POINT('Ctrl Pts',(-0.533501897135712,-0.0762225747374254,
-0.989110885965947));
#13030=CARTESIAN_POINT('Ctrl Pts',(-0.529268075276156,-0.0928409665394227,
-0.991396466802469));
#13031=CARTESIAN_POINT('Ctrl Pts',(-0.511762781179147,-0.144299303100741,
-1.00061845128527));
#13032=CARTESIAN_POINT('Ctrl Pts',(-0.493462957200432,-0.177024326825049,
-1.0099536580922));
#13033=CARTESIAN_POINT('Ctrl Pts',(-0.45280897844858,-0.227269801620063,
-1.02876878445619));
#13034=CARTESIAN_POINT('Ctrl Pts',(-0.425554672694337,-0.251265615809407,
-1.04048957871266));
#13035=CARTESIAN_POINT('Ctrl Pts',(-0.3787731215897,-0.279889827963178,
-1.05829506364875));
#13036=CARTESIAN_POINT('Ctrl Pts',(-0.354166711873529,-0.290879136862659,
-1.06688848765783));
#13037=CARTESIAN_POINT('Ctrl Pts',(-0.302426893214944,-0.305251990234488,
-1.08269251410343));
#13038=CARTESIAN_POINT('Ctrl Pts',(-0.275287440920027,-0.308638795020976,
-1.0898803575765));
#13039=CARTESIAN_POINT('Ctrl Pts',(-0.224855950742601,-0.308638795020976,
-1.10139101611326));
#13040=CARTESIAN_POINT('Ctrl Pts',(-0.19728546073067,-0.305251990234488,
-1.10669035995599));
#13041=CARTESIAN_POINT('Ctrl Pts',(-0.143812384801039,-0.290879136862659,
-1.11490049012186));
#13042=CARTESIAN_POINT('Ctrl Pts',(-0.117914228755037,-0.279889827963178,
-1.1178344036749));
#13043=CARTESIAN_POINT('Ctrl Pts',(-0.0680399972366989,-0.251265615809407,
-1.12208997038458));
#13044=CARTESIAN_POINT('Ctrl Pts',(-0.0383992541984084,-0.227269801620063,
-1.12335509974011));
#13045=CARTESIAN_POINT('Ctrl Pts',(0.00639229239215326,-0.177024326825049,
-1.12404235695137));
#13046=CARTESIAN_POINT('Ctrl Pts',(0.0269302585198977,-0.144299303100741,
-1.12357162229597));
#13047=CARTESIAN_POINT('Ctrl Pts',(0.04670325263426,-0.0928409665394228,
-1.12285816383385));
#13048=CARTESIAN_POINT('Ctrl Pts',(0.0515094706813703,-0.0762225747374255,
-1.12263591311425));
#13049=CARTESIAN_POINT('Ctrl Pts',(0.0548532617164176,-0.0595300000000001,
-1.12247250791414));
#13050=CARTESIAN_POINT('',(0.437601487681057,-0.05953,-1.03511272300331));
#13051=CARTESIAN_POINT('Origin',(0.,-0.05953,0.));
#13052=CARTESIAN_POINT('',(0.911784794170997,-0.05953,-0.656964154625313));
#13053=CARTESIAN_POINT('Ctrl Pts',(0.437601487681056,-0.0595300000000001,
-1.03511272300331));
#13054=CARTESIAN_POINT('Ctrl Pts',(0.440685038163619,-0.0762225747374255,
-1.03380912944435));
#13055=CARTESIAN_POINT('Ctrl Pts',(0.445111721969657,-0.0928409665394228,
-1.03192403056628));
#13056=CARTESIAN_POINT('Ctrl Pts',(0.463236132117164,-0.144299303100741,
-1.0239876538093));
#13057=CARTESIAN_POINT('Ctrl Pts',(0.481944444320713,-0.177024326825049,
-1.01550068154148));
#13058=CARTESIAN_POINT('Ctrl Pts',(0.522002043615455,-0.227269801620064,
-0.995447160474328));
#13059=CARTESIAN_POINT('Ctrl Pts',(0.548158511259203,-0.251265615809407,
-0.981446681891443));
#13060=CARTESIAN_POINT('Ctrl Pts',(0.591247219971725,-0.279889827963178,
-0.955972930713954));
#13061=CARTESIAN_POINT('Ctrl Pts',(0.613307674922609,-0.290879136862659,
-0.942092777160053));
#13062=CARTESIAN_POINT('Ctrl Pts',(0.657923009631182,-0.305251990234487,
-0.91149460735272));
#13063=CARTESIAN_POINT('Ctrl Pts',(0.680463863683393,-0.308638795020976,
-0.894757676234429));
#13064=CARTESIAN_POINT('Ctrl Pts',(0.720906778729542,-0.308638795020976,
-0.862505527716294));
#13065=CARTESIAN_POINT('Ctrl Pts',(0.742239891936899,-0.305251990234488,
-0.844254137480381));
#13066=CARTESIAN_POINT('Ctrl Pts',(0.781998747691872,-0.290879136862659,
-0.80756613568454));
#13067=CARTESIAN_POINT('Ctrl Pts',(0.800439809856112,-0.279889827963178,
-0.789147407129765));
#13068=CARTESIAN_POINT('Ctrl Pts',(0.834863020612702,-0.251265615809407,
-0.752807465209441));
#13069=CARTESIAN_POINT('Ctrl Pts',(0.854332839576145,-0.227269801620064,
-0.73042219438957));
#13070=CARTESIAN_POINT('Ctrl Pts',(0.882797231409153,-0.177024326825049,
-0.695831250979106));
#13071=CARTESIAN_POINT('Ctrl Pts',(0.895234408667242,-0.144299303100741,
-0.679480524217551));
#13072=CARTESIAN_POINT('Ctrl Pts',(0.907004864562642,-0.0928409665394228,
-0.663576540841106));
#13073=CARTESIAN_POINT('Ctrl Pts',(0.909827729890942,-0.0762225747374256,
-0.659680317203144));
#13074=CARTESIAN_POINT('Ctrl Pts',(0.911784794170998,-0.0595300000000001,
-0.656964154625312));
#13075=CARTESIAN_POINT('',(1.08212377959455,-0.05953,-0.303251606722892));
#13076=CARTESIAN_POINT('Origin',(0.,-0.05953,0.));
#13077=CARTESIAN_POINT('',(1.08212377959455,-0.05953,0.303251606722892));
#13078=CARTESIAN_POINT('Ctrl Pts',(1.08212377959455,-0.0595300000000001,
-0.303251606722892));
#13079=CARTESIAN_POINT('Ctrl Pts',(1.0830271513892,-0.0762225747374255,
-0.300028012588062));
#13080=CARTESIAN_POINT('Ctrl Pts',(1.08431331394788,-0.0928409665394228,
-0.2953917518996));
#13081=CARTESIAN_POINT('Ctrl Pts',(1.08940878963422,-0.144299303100741,
-0.276273267473431));
#13082=CARTESIAN_POINT('Ctrl Pts',(1.09443784939331,-0.177024326825049,
-0.256354979351213));
#13083=CARTESIAN_POINT('Ctrl Pts',(1.10373487993589,-0.227269801620064,
-0.212533521233765));
#13084=CARTESIAN_POINT('Ctrl Pts',(1.10909715583869,-0.251265615809407,
-0.183354415742157));
#13085=CARTESIAN_POINT('Ctrl Pts',(1.1160463456491,-0.279889827963178,-0.133783682657561));
#13086=CARTESIAN_POINT('Ctrl Pts',(1.11894887330541,-0.290879136862659,
-0.107881990270302));
#13087=CARTESIAN_POINT('Ctrl Pts',(1.12284346704144,-0.305251990234488,
-0.0539226701638766));
#13088=CARTESIAN_POINT('Ctrl Pts',(1.123812,-0.308638795020976,-0.025864214957475));
#13089=CARTESIAN_POINT('Ctrl Pts',(1.123812,-0.308638795020976,0.025864214957475));
#13090=CARTESIAN_POINT('Ctrl Pts',(1.12284346704144,-0.305251990234488,
0.0539226701638766));
#13091=CARTESIAN_POINT('Ctrl Pts',(1.11894887330541,-0.290879136862659,
0.107881990270302));
#13092=CARTESIAN_POINT('Ctrl Pts',(1.1160463456491,-0.279889827963178,0.133783682657561));
#13093=CARTESIAN_POINT('Ctrl Pts',(1.10909715583869,-0.251265615809407,
0.183354415742157));
#13094=CARTESIAN_POINT('Ctrl Pts',(1.10373487993589,-0.227269801620064,
0.212533521233765));
#13095=CARTESIAN_POINT('Ctrl Pts',(1.09443784939331,-0.177024326825049,
0.256354979351213));
#13096=CARTESIAN_POINT('Ctrl Pts',(1.08940878963422,-0.144299303100741,
0.276273267473431));
#13097=CARTESIAN_POINT('Ctrl Pts',(1.08431331394788,-0.0928409665394228,
0.2953917518996));
#13098=CARTESIAN_POINT('Ctrl Pts',(1.0830271513892,-0.0762225747374255,
0.300028012588062));
#13099=CARTESIAN_POINT('Ctrl Pts',(1.08212377959455,-0.0595300000000001,
0.303251606722892));
#13100=CARTESIAN_POINT('Origin',(0.,-0.05953,0.));
#13101=CARTESIAN_POINT('Origin',(0.,-0.05953,0.));
#13102=CARTESIAN_POINT('',(0.0589974094846122,-0.05953,1.07456964270265));
#13103=CARTESIAN_POINT('Origin',(0.,-0.05953,0.));
#13104=CARTESIAN_POINT('Origin',(-0.244773027351946,-0.05953,1.07242070340001));
#13105=CARTESIAN_POINT('Origin',(-0.244773027351946,0.,1.07242070340001));
#13106=CARTESIAN_POINT('',(-0.519393123750572,-0.05953,0.942555777842682));
#13107=CARTESIAN_POINT('Ctrl Pts',(-0.519393123750572,-0.05953,0.942555777842682));
#13108=CARTESIAN_POINT('Ctrl Pts',(-0.513714466572041,-0.0925528133349865,
0.945684988399766));
#13109=CARTESIAN_POINT('Ctrl Pts',(-0.503136848051455,-0.124911173756694,
0.951483858396181));
#13110=CARTESIAN_POINT('Ctrl Pts',(-0.47593627990192,-0.177924977804098,
0.965323333309091));
#13111=CARTESIAN_POINT('Ctrl Pts',(-0.460931856495794,-0.199697230012983,
0.972669835243841));
#13112=CARTESIAN_POINT('Ctrl Pts',(-0.426157505475872,-0.237895043532788,
0.988400002689705));
#13113=CARTESIAN_POINT('Ctrl Pts',(-0.406380688682952,-0.254319232363049,
0.996771768218699));
#13114=CARTESIAN_POINT('Ctrl Pts',(-0.364750145543744,-0.28018331644634,
1.01272583306292));
#13115=CARTESIAN_POINT('Ctrl Pts',(-0.340838910881557,-0.29104845371857,
1.02112815447116));
#13116=CARTESIAN_POINT('Ctrl Pts',(-0.290495481564827,-0.30527573347708,
1.036574285215));
#13117=CARTESIAN_POINT('Ctrl Pts',(-0.264056468041074,-0.308638795020976,
1.04359501395068));
#13118=CARTESIAN_POINT('Ctrl Pts',(-0.214892249704082,-0.308638795020976,
1.05481642595959));
#13119=CARTESIAN_POINT('Ctrl Pts',(-0.188025341585962,-0.30527573347708,
1.05996242598502));
#13120=CARTESIAN_POINT('Ctrl Pts',(-0.135965654106109,-0.29104845371857,
1.06788913840721));
#13121=CARTESIAN_POINT('Ctrl Pts',(-0.110776745452494,-0.28018331644634,
1.07069360430242));
#13122=CARTESIAN_POINT('Ctrl Pts',(-0.0663467128214646,-0.254319232363049,
1.07438230428002));
#13123=CARTESIAN_POINT('Ctrl Pts',(-0.0448960436540983,-0.237895043532788,
1.07542044338697));
#13124=CARTESIAN_POINT('Ctrl Pts',(-0.00674037211528124,-0.199697230012983,
1.07633607767727));
#13125=CARTESIAN_POINT('Ctrl Pts',(0.00996567398334777,-0.177924977804098,
1.07622728347683));
#13126=CARTESIAN_POINT('Ctrl Pts',(0.0404772621979741,-0.124911173756694,
1.07556023164702));
#13127=CARTESIAN_POINT('Ctrl Pts',(0.0525234025782719,-0.0925528133349865,
1.07492508698591));
#13128=CARTESIAN_POINT('Ctrl Pts',(0.0589974094846124,-0.05953,1.07456964270265));
#13129=CARTESIAN_POINT('Origin',(-0.244773027351946,-0.05953,1.07242070340001));
#13130=CARTESIAN_POINT('Origin',(0.,-0.05953,0.));
#13131=CARTESIAN_POINT('',(-0.803348093619616,-0.05953,0.716109245731214));
#13132=CARTESIAN_POINT('Origin',(0.,-0.05953,0.));
#13133=CARTESIAN_POINT('Origin',(-0.991065754692661,-0.05953,0.477272113029314));
#13134=CARTESIAN_POINT('Origin',(-0.991065754692661,0.,0.477272113029314));
#13135=CARTESIAN_POINT('',(-1.06075609691358,-0.05953,0.181596019242328));
#13136=CARTESIAN_POINT('Ctrl Pts',(-1.06075609691358,-0.05953,0.181596019242328));
#13137=CARTESIAN_POINT('Ctrl Pts',(-1.05966202740332,-0.0925528133349865,
0.187986803072856));
#13138=CARTESIAN_POINT('Ctrl Pts',(-1.05760072925372,-0.124911173756694,
0.199872254546857));
#13139=CARTESIAN_POINT('Ctrl Pts',(-1.05146158959546,-0.177924977804098,
0.22976728653846));
#13140=CARTESIAN_POINT('Ctrl Pts',(-1.04785021111757,-0.199697230012983,
0.246078686169301));
#13141=CARTESIAN_POINT('Ctrl Pts',(-1.03846709802406,-0.237895043532788,
0.283073967563097));
#13142=CARTESIAN_POINT('Ctrl Pts',(-1.03268176429485,-0.254319232363049,
0.303755815985685));
#13143=CARTESIAN_POINT('Ctrl Pts',(-1.01919893537026,-0.28018331644634,
0.346251081972725));
#13144=CARTESIAN_POINT('Ctrl Pts',(-1.01085972381132,-0.29104845371857,
0.370184399726282));
#13145=CARTESIAN_POINT('Ctrl Pts',(-0.99154738033959,-0.30527573347708,
0.419174982698463));
#13146=CARTESIAN_POINT('Ctrl Pts',(-0.980551951791748,-0.308638795020976,
0.444223188605045));
#13147=CARTESIAN_POINT('Ctrl Pts',(-0.958671816228589,-0.308638795020976,
0.489657758261848));
#13148=CARTESIAN_POINT('Ctrl Pts',(-0.945943877838127,-0.30527573347708,
0.51387163140139));
#13149=CARTESIAN_POINT('Ctrl Pts',(-0.91968254693063,-0.29104845371857,
0.559515758398093));
#13150=CARTESIAN_POINT('Ctrl Pts',(-0.906170138993533,-0.28018331644634,
0.580957796077825));
#13151=CARTESIAN_POINT('Ctrl Pts',(-0.8813524085237,-0.254319232363049,
0.617994461173994));
#13152=CARTESIAN_POINT('Ctrl Pts',(-0.868789784891799,-0.237895043532788,
0.635412538795143));
#13153=CARTESIAN_POINT('Ctrl Pts',(-0.845715984518854,-0.199697230012983,
0.66581473268113));
#13154=CARTESIAN_POINT('Ctrl Pts',(-0.835214876415962,-0.177924977804098,
0.678808213394124));
#13155=CARTESIAN_POINT('Ctrl Pts',(-0.815669690204649,-0.124911173756694,
0.702247233627224));
#13156=CARTESIAN_POINT('Ctrl Pts',(-0.807662468433796,-0.0925528133349865,
0.711269279199861));
#13157=CARTESIAN_POINT('Ctrl Pts',(-0.803348093619616,-0.05953,0.716109245731214));
#13158=CARTESIAN_POINT('Origin',(-0.991065754692661,-0.05953,0.477272113029314));
#13159=CARTESIAN_POINT('Origin',(0.,-0.05953,0.));
#13160=CARTESIAN_POINT('',(-1.076188,-0.05953,1.31795018948079E-16));
#13161=CARTESIAN_POINT('Origin',(0.,-0.05953,0.));
#13162=CARTESIAN_POINT('',(-1.06075609691358,-0.05953,-0.181596019242328));
#13163=CARTESIAN_POINT('Origin',(0.,-0.05953,0.));
#13164=CARTESIAN_POINT('Origin',(-0.991065754692661,-0.05953,-0.477272113029314));
#13165=CARTESIAN_POINT('Origin',(-0.991065754692661,0.,-0.477272113029314));
#13166=CARTESIAN_POINT('',(-0.803348093619616,-0.05953,-0.716109245731215));
#13167=CARTESIAN_POINT('Ctrl Pts',(-0.803348093619616,-0.05953,-0.716109245731215));
#13168=CARTESIAN_POINT('Ctrl Pts',(-0.807662468433795,-0.0925528133349865,
-0.711269279199862));
#13169=CARTESIAN_POINT('Ctrl Pts',(-0.815669690204649,-0.124911173756694,
-0.702247233627224));
#13170=CARTESIAN_POINT('Ctrl Pts',(-0.835214876415962,-0.177924977804098,
-0.678808213394124));
#13171=CARTESIAN_POINT('Ctrl Pts',(-0.845715984518854,-0.199697230012983,
-0.66581473268113));
#13172=CARTESIAN_POINT('Ctrl Pts',(-0.868789784891799,-0.237895043532788,
-0.635412538795143));
#13173=CARTESIAN_POINT('Ctrl Pts',(-0.8813524085237,-0.254319232363049,
-0.617994461173994));
#13174=CARTESIAN_POINT('Ctrl Pts',(-0.906170138993533,-0.28018331644634,
-0.580957796077826));
#13175=CARTESIAN_POINT('Ctrl Pts',(-0.91968254693063,-0.29104845371857,
-0.559515758398093));
#13176=CARTESIAN_POINT('Ctrl Pts',(-0.945943877838127,-0.30527573347708,
-0.51387163140139));
#13177=CARTESIAN_POINT('Ctrl Pts',(-0.958671816228589,-0.308638795020976,
-0.489657758261848));
#13178=CARTESIAN_POINT('Ctrl Pts',(-0.980551951791748,-0.308638795020976,
-0.444223188605045));
#13179=CARTESIAN_POINT('Ctrl Pts',(-0.99154738033959,-0.30527573347708,
-0.419174982698463));
#13180=CARTESIAN_POINT('Ctrl Pts',(-1.01085972381132,-0.29104845371857,
-0.370184399726282));
#13181=CARTESIAN_POINT('Ctrl Pts',(-1.01919893537026,-0.28018331644634,
-0.346251081972725));
#13182=CARTESIAN_POINT('Ctrl Pts',(-1.03268176429485,-0.254319232363049,
-0.303755815985685));
#13183=CARTESIAN_POINT('Ctrl Pts',(-1.03846709802406,-0.237895043532788,
-0.283073967563097));
#13184=CARTESIAN_POINT('Ctrl Pts',(-1.04785021111757,-0.199697230012983,
-0.246078686169302));
#13185=CARTESIAN_POINT('Ctrl Pts',(-1.05146158959546,-0.177924977804098,
-0.229767286538461));
#13186=CARTESIAN_POINT('Ctrl Pts',(-1.05760072925372,-0.124911173756694,
-0.199872254546858));
#13187=CARTESIAN_POINT('Ctrl Pts',(-1.05966202740332,-0.0925528133349864,
-0.187986803072857));
#13188=CARTESIAN_POINT('Ctrl Pts',(-1.06075609691358,-0.05953,-0.181596019242328));
#13189=CARTESIAN_POINT('Origin',(-0.991065754692661,-0.05953,-0.477272113029314));
#13190=CARTESIAN_POINT('Origin',(0.,-0.05953,0.));
#13191=CARTESIAN_POINT('',(-0.519393123750572,-0.05953,-0.942555777842682));
#13192=CARTESIAN_POINT('Origin',(0.,-0.05953,0.));
#13193=CARTESIAN_POINT('Origin',(-0.244773027351946,-0.05953,-1.07242070340001));
#13194=CARTESIAN_POINT('Origin',(-0.244773027351946,0.,-1.07242070340001));
#13195=CARTESIAN_POINT('',(0.0589974094846125,-0.05953,-1.07456964270265));
#13196=CARTESIAN_POINT('Ctrl Pts',(0.0589974094846127,-0.05953,-1.07456964270265));
#13197=CARTESIAN_POINT('Ctrl Pts',(0.0525234025782722,-0.0925528133349865,
-1.07492508698591));
#13198=CARTESIAN_POINT('Ctrl Pts',(0.0404772621979744,-0.124911173756694,
-1.07556023164702));
#13199=CARTESIAN_POINT('Ctrl Pts',(0.0099656739833481,-0.177924977804098,
-1.07622728347683));
#13200=CARTESIAN_POINT('Ctrl Pts',(-0.00674037211528096,-0.199697230012983,
-1.07633607767727));
#13201=CARTESIAN_POINT('Ctrl Pts',(-0.044896043654098,-0.237895043532788,
-1.07542044338697));
#13202=CARTESIAN_POINT('Ctrl Pts',(-0.0663467128214644,-0.254319232363049,
-1.07438230428002));
#13203=CARTESIAN_POINT('Ctrl Pts',(-0.110776745452493,-0.28018331644634,
-1.07069360430242));
#13204=CARTESIAN_POINT('Ctrl Pts',(-0.135965654106109,-0.29104845371857,
-1.06788913840721));
#13205=CARTESIAN_POINT('Ctrl Pts',(-0.188025341585962,-0.30527573347708,
-1.05996242598502));
#13206=CARTESIAN_POINT('Ctrl Pts',(-0.214892249704082,-0.308638795020976,
-1.05481642595959));
#13207=CARTESIAN_POINT('Ctrl Pts',(-0.264056468041074,-0.308638795020976,
-1.04359501395068));
#13208=CARTESIAN_POINT('Ctrl Pts',(-0.290495481564827,-0.30527573347708,
-1.036574285215));
#13209=CARTESIAN_POINT('Ctrl Pts',(-0.340838910881557,-0.291048453718569,
-1.02112815447116));
#13210=CARTESIAN_POINT('Ctrl Pts',(-0.364750145543744,-0.28018331644634,
-1.01272583306292));
#13211=CARTESIAN_POINT('Ctrl Pts',(-0.406380688682952,-0.254319232363049,
-0.996771768218699));
#13212=CARTESIAN_POINT('Ctrl Pts',(-0.426157505475872,-0.237895043532788,
-0.988400002689705));
#13213=CARTESIAN_POINT('Ctrl Pts',(-0.460931856495794,-0.199697230012983,
-0.972669835243841));
#13214=CARTESIAN_POINT('Ctrl Pts',(-0.475936279901919,-0.177924977804098,
-0.965323333309091));
#13215=CARTESIAN_POINT('Ctrl Pts',(-0.503136848051454,-0.124911173756694,
-0.951483858396181));
#13216=CARTESIAN_POINT('Ctrl Pts',(-0.513714466572041,-0.0925528133349865,
-0.945684988399766));
#13217=CARTESIAN_POINT('Ctrl Pts',(-0.519393123750572,-0.05953,-0.942555777842682));
#13218=CARTESIAN_POINT('Origin',(-0.244773027351946,-0.05953,-1.07242070340001));
#13219=CARTESIAN_POINT('Origin',(0.,-0.05953,0.));
#13220=CARTESIAN_POINT('',(0.413083465285518,-0.05953,-0.993751811093549));
#13221=CARTESIAN_POINT('Origin',(0.,-0.05953,0.));
#13222=CARTESIAN_POINT('Origin',(0.685838782044607,-0.05953,-0.860014630714833));
#13223=CARTESIAN_POINT('Origin',(0.685838782044607,0.,-0.860014630714833));
#13224=CARTESIAN_POINT('',(0.876916659919095,-0.05953,-0.623857181492959));
#13225=CARTESIAN_POINT('Ctrl Pts',(0.876916659919095,-0.05953,-0.623857181492958));
#13226=CARTESIAN_POINT('Ctrl Pts',(0.873158080166742,-0.0925528133349865,
-0.62914037979579));
#13227=CARTESIAN_POINT('Ctrl Pts',(0.866144010579847,-0.124911173756694,
-0.638954437806245));
#13228=CARTESIAN_POINT('Ctrl Pts',(0.847641868610495,-0.177924977804098,
-0.663225258065736));
#13229=CARTESIAN_POINT('Ctrl Pts',(0.837310877969633,-0.199697230012983,
-0.676354402927683));
#13230=CARTESIAN_POINT('Ctrl Pts',(0.81280533416753,-0.237895043532788,
-0.705614819529209));
#13231=CARTESIAN_POINT('Ctrl Pts',(0.798619410861634,-0.254319232363049,
-0.721738358858166));
#13232=CARTESIAN_POINT('Ctrl Pts',(0.768033796848072,-0.28018331644634,
-0.754175290318038));
#13233=CARTESIAN_POINT('Ctrl Pts',(0.750136149454208,-0.29104845371857,
-0.772120216227122));
#13234=CARTESIAN_POINT('Ctrl Pts',(0.711480111898423,-0.30527573347708,
-0.807879894508811));
#13235=CARTESIAN_POINT('Ctrl Pts',(0.690705563850638,-0.308638795020976,
-0.825676810575913));
#13236=CARTESIAN_POINT('Ctrl Pts',(0.651278921914856,-0.308638795020976,
-0.857118508332695));
#13237=CARTESIAN_POINT('Ctrl Pts',(0.629305439856167,-0.30527573347708,
-0.873412008702649));
#13238=CARTESIAN_POINT('Ctrl Pts',(0.585840553788742,-0.29104845371857,
-0.903141581680914));
#13239=CARTESIAN_POINT('Ctrl Pts',(0.564362943424239,-0.28018331644634,
-0.916597376014514));
#13240=CARTESIAN_POINT('Ctrl Pts',(0.525933334162556,-0.254319232363049,
-0.939198248544427));
#13241=CARTESIAN_POINT('Ctrl Pts',(0.507057380724533,-0.237895043532788,
-0.949440676105255));
#13242=CARTESIAN_POINT('Ctrl Pts',(0.473077587363686,-0.199697230012983,
-0.966820759530997));
#13243=CARTESIAN_POINT('Ctrl Pts',(0.457978755888596,-0.177924977804098,
-0.973971221090534));
#13244=CARTESIAN_POINT('Ctrl Pts',(0.430199341854858,-0.124911173756694,
-0.986608710139579));
#13245=CARTESIAN_POINT('Ctrl Pts',(0.419070565453384,-0.0925528133349865,
-0.991263089003441));
#13246=CARTESIAN_POINT('Ctrl Pts',(0.413083465285518,-0.05953,-0.993751811093549));
#13247=CARTESIAN_POINT('Origin',(0.685838782044607,-0.05953,-0.860014630714833));
#13248=CARTESIAN_POINT('Origin',(0.,-0.208355,0.));
#13249=CARTESIAN_POINT('',(-1.076188,-0.35718,1.31795018948079E-16));
#13250=CARTESIAN_POINT('Origin',(0.,-0.35718,0.));
#13251=CARTESIAN_POINT('',(-1.076188,-0.208355,1.31795018948079E-16));
#13252=CARTESIAN_POINT('',(1.03449977959455,-0.05953,0.296632461748266));
#13253=CARTESIAN_POINT('Origin',(0.,-0.05953,0.));
#13254=CARTESIAN_POINT('',(1.03449977959455,-0.05953,-0.296632461748266));
#13255=CARTESIAN_POINT('Ctrl Pts',(1.03449977959455,-0.05953,0.296632461748267));
#13256=CARTESIAN_POINT('Ctrl Pts',(1.03628691421076,-0.0925528133349865,
0.290399865505497));
#13257=CARTESIAN_POINT('Ctrl Pts',(1.03958665287714,-0.124911173756694,
0.278797079997872));
#13258=CARTESIAN_POINT('Ctrl Pts',(1.0470264474309,-0.177924977804098,0.249198913998601));
#13259=CARTESIAN_POINT('Ctrl Pts',(1.05084995891418,-0.199697230012983,
0.232935932341942));
#13260=CARTESIAN_POINT('Ctrl Pts',(1.05844771715377,-0.237895043532788,
0.195533155353269));
#13261=CARTESIAN_POINT('Ctrl Pts',(1.06220882929878,-0.254319232363049,
0.17438929156337));
#13262=CARTESIAN_POINT('Ctrl Pts',(1.06849922508772,-0.28018331644634,0.130252399648131));
#13263=CARTESIAN_POINT('Ctrl Pts',(1.07137013248666,-0.29104845371857,0.105070977154072));
#13264=CARTESIAN_POINT('Ctrl Pts',(1.07522652957392,-0.30527573347708,0.0525526752791107));
#13265=CARTESIAN_POINT('Ctrl Pts',(1.076188,-0.308638795020976,0.025214283908933));
#13266=CARTESIAN_POINT('Ctrl Pts',(1.076188,-0.308638795020976,-0.025214283908933));
#13267=CARTESIAN_POINT('Ctrl Pts',(1.07522652957392,-0.30527573347708,-0.0525526752791107));
#13268=CARTESIAN_POINT('Ctrl Pts',(1.07137013248666,-0.29104845371857,-0.105070977154072));
#13269=CARTESIAN_POINT('Ctrl Pts',(1.06849922508772,-0.28018331644634,-0.130252399648131));
#13270=CARTESIAN_POINT('Ctrl Pts',(1.06220882929878,-0.254319232363049,
-0.17438929156337));
#13271=CARTESIAN_POINT('Ctrl Pts',(1.05844771715377,-0.237895043532788,
-0.195533155353269));
#13272=CARTESIAN_POINT('Ctrl Pts',(1.05084995891418,-0.199697230012983,
-0.232935932341942));
#13273=CARTESIAN_POINT('Ctrl Pts',(1.0470264474309,-0.177924977804098,-0.249198913998601));
#13274=CARTESIAN_POINT('Ctrl Pts',(1.03958665287714,-0.124911173756694,
-0.278797079997872));
#13275=CARTESIAN_POINT('Ctrl Pts',(1.03628691421076,-0.0925528133349865,
-0.290399865505497));
#13276=CARTESIAN_POINT('Ctrl Pts',(1.03449977959455,-0.05953,-0.296632461748267));
#13277=CARTESIAN_POINT('Origin',(0.,-0.05953,0.));
#13278=CARTESIAN_POINT('Origin',(0.,-0.05953,0.));
#13279=CARTESIAN_POINT('Origin',(1.1,-0.05953,0.));
#13280=CARTESIAN_POINT('Origin',(1.1,0.,0.));
#13281=CARTESIAN_POINT('Origin',(1.1,-0.05953,0.));
#13282=CARTESIAN_POINT('Origin',(0.,-0.35718,0.));
#13283=CARTESIAN_POINT('Origin',(0.,-0.05953,0.));
#13284=CARTESIAN_POINT('',(0.,0.,0.));
#13285=CARTESIAN_POINT('Origin',(1.119765,0.495,0.));
#13286=CARTESIAN_POINT('',(-1.119765,0.495,-1.37131662304724E-16));
#13287=CARTESIAN_POINT('Origin',(0.,0.495,0.));
#13288=CARTESIAN_POINT('',(-1.085235,0.495,-1.32902956907268E-16));
#13289=CARTESIAN_POINT('Origin',(0.,0.495,0.));
#13290=CARTESIAN_POINT('Origin',(0.,0.4575,0.));
#13291=CARTESIAN_POINT('',(-1.119765,0.42,-1.37131662304724E-16));
#13292=CARTESIAN_POINT('Origin',(0.,0.42,0.));
#13293=CARTESIAN_POINT('',(-1.119765,0.4575,-1.37131662304724E-16));
#13294=CARTESIAN_POINT('Origin',(1.085235,0.42,0.));
#13295=CARTESIAN_POINT('',(-1.085235,0.42,-1.32902956907268E-16));
#13296=CARTESIAN_POINT('Origin',(0.,0.42,0.));
#13297=CARTESIAN_POINT('Origin',(0.,0.4575,0.));
#13298=CARTESIAN_POINT('',(-1.085235,0.4575,-1.32902956907268E-16));
#13299=CARTESIAN_POINT('Origin',(1.119765,-0.42,0.));
#13300=CARTESIAN_POINT('',(-1.119765,-0.42,-1.37131662304724E-16));
#13301=CARTESIAN_POINT('Origin',(0.,-0.42,0.));
#13302=CARTESIAN_POINT('',(-1.085235,-0.42,-1.32902956907268E-16));
#13303=CARTESIAN_POINT('Origin',(0.,-0.42,0.));
#13304=CARTESIAN_POINT('Origin',(0.,-0.4575,0.));
#13305=CARTESIAN_POINT('',(-1.119765,-0.495,-1.37131662304724E-16));
#13306=CARTESIAN_POINT('Origin',(0.,-0.495,0.));
#13307=CARTESIAN_POINT('',(-1.119765,-0.4575,-1.37131662304724E-16));
#13308=CARTESIAN_POINT('Origin',(1.085235,-0.495,0.));
#13309=CARTESIAN_POINT('',(-1.085235,-0.495,-1.32902956907268E-16));
#13310=CARTESIAN_POINT('Origin',(0.,-0.495,0.));
#13311=CARTESIAN_POINT('Origin',(0.,-0.4575,0.));
#13312=CARTESIAN_POINT('',(-1.085235,-0.4575,-1.32902956907268E-16));
#13313=CARTESIAN_POINT('',(0.,0.,0.));
#13314=CARTESIAN_POINT('',(0.,0.,0.));
#13315=CARTESIAN_POINT('',(0.,0.,0.));
#13316=CARTESIAN_POINT('',(0.,0.,0.));
#13317=CARTESIAN_POINT('',(0.,0.,0.));
#13318=CARTESIAN_POINT('',(0.,0.,0.));
#13319=CARTESIAN_POINT('',(0.,0.,0.));
#13320=CARTESIAN_POINT('Origin',(0.,0.,0.));
#13321=CARTESIAN_POINT('',(-1.63531,-0.410863395882378,-2.00267715711366E-16));
#13322=CARTESIAN_POINT('',(-2.00267715711366E-16,-0.410863395882378,1.63531));
#13323=CARTESIAN_POINT('Origin',(0.,-0.410863395882378,0.));
#13324=CARTESIAN_POINT('Origin',(0.,-0.410863395882378,0.));
#13325=CARTESIAN_POINT('',(-2.00267715711366E-16,0.410863395882378,1.63531));
#13326=CARTESIAN_POINT('Origin',(-2.05128338857182E-16,0.,1.675));
#13327=CARTESIAN_POINT('',(-1.63531,0.410863395882378,2.00267715711366E-16));
#13328=CARTESIAN_POINT('Origin',(0.,0.410863395882378,0.));
#13329=CARTESIAN_POINT('Origin',(0.,0.410863395882378,0.));
#13330=CARTESIAN_POINT('Origin',(0.,0.,0.));
#13331=CARTESIAN_POINT('',(-1.63531,0.7,-2.00267715711366E-16));
#13332=CARTESIAN_POINT('',(-1.63531,0.,-2.00267715711366E-16));
#13333=CARTESIAN_POINT('Origin',(0.,0.7,0.));
#13334=CARTESIAN_POINT('Origin',(0.,0.,0.));
#13335=CARTESIAN_POINT('',(-1.,-0.6,-1.22464679914735E-16));
#13336=CARTESIAN_POINT('Origin',(0.,-0.6,0.));
#13337=CARTESIAN_POINT('',(-1.,0.6,-1.22464679914735E-16));
#13338=CARTESIAN_POINT('',(-1.,0.,-1.22464679914735E-16));
#13339=CARTESIAN_POINT('Origin',(0.,0.6,0.));
#13340=CARTESIAN_POINT('Origin',(0.,0.65,0.));
#13341=CARTESIAN_POINT('',(-1.1,0.7,-1.34711147906209E-16));
#13342=CARTESIAN_POINT('',(-1.05,0.65,-1.28587913910472E-16));
#13343=CARTESIAN_POINT('Origin',(0.,0.7,0.));
#13344=CARTESIAN_POINT('Origin',(1.63531,0.7,0.));
#13345=CARTESIAN_POINT('Origin',(0.,0.,0.));
#13346=CARTESIAN_POINT('',(-1.63531,-0.7,-2.00267715711366E-16));
#13347=CARTESIAN_POINT('Origin',(0.,-0.7,0.));
#13348=CARTESIAN_POINT('',(-1.63531,0.,-2.00267715711366E-16));
#13349=CARTESIAN_POINT('Origin',(1.1,-0.7,0.));
#13350=CARTESIAN_POINT('',(-1.1,-0.7,-1.34711147906209E-16));
#13351=CARTESIAN_POINT('Origin',(0.,-0.7,0.));
#13352=CARTESIAN_POINT('Origin',(0.,-0.65,0.));
#13353=CARTESIAN_POINT('',(-1.05,-0.65,-1.28587913910472E-16));
#13354=CARTESIAN_POINT('',(0.,0.,0.));
#13355=CARTESIAN_POINT('Origin',(0.,0.,0.));
#13356=CARTESIAN_POINT('',(-1.71469,0.410863395882378,-2.09988962002998E-16));
#13357=CARTESIAN_POINT('',(-2.09988962002998E-16,0.410863395882378,1.71469));
#13358=CARTESIAN_POINT('Origin',(0.,0.410863395882378,0.));
#13359=CARTESIAN_POINT('Origin',(0.,0.410863395882378,0.));
#13360=CARTESIAN_POINT('',(-2.09988962002998E-16,-0.410863395882378,1.71469));
#13361=CARTESIAN_POINT('Origin',(-2.05128338857182E-16,0.,1.675));
#13362=CARTESIAN_POINT('',(-1.71469,-0.410863395882378,2.09988962002998E-16));
#13363=CARTESIAN_POINT('Origin',(0.,-0.410863395882378,0.));
#13364=CARTESIAN_POINT('Origin',(0.,-0.410863395882378,0.));
#13365=CARTESIAN_POINT('Origin',(0.,0.,0.));
#13366=CARTESIAN_POINT('',(-1.71469,-0.7,-2.09988962002998E-16));
#13367=CARTESIAN_POINT('Origin',(0.,-0.7,0.));
#13368=CARTESIAN_POINT('',(-1.71469,0.,-2.09988962002998E-16));
#13369=CARTESIAN_POINT('Origin',(2.25,0.7,0.));
#13370=CARTESIAN_POINT('',(-2.25,0.7,-2.75545529808154E-16));
#13371=CARTESIAN_POINT('Origin',(0.,0.7,0.));
#13372=CARTESIAN_POINT('',(-1.71469,0.7,-2.09988962002998E-16));
#13373=CARTESIAN_POINT('Origin',(0.,0.7,0.));
#13374=CARTESIAN_POINT('Origin',(0.,0.65,0.));
#13375=CARTESIAN_POINT('',(-2.35,0.6,-2.87791997799628E-16));
#13376=CARTESIAN_POINT('Origin',(0.,0.6,0.));
#13377=CARTESIAN_POINT('',(-2.3,0.65,-2.81668763803891E-16));
#13378=CARTESIAN_POINT('Origin',(0.,0.,0.));
#13379=CARTESIAN_POINT('',(-2.35,-0.6,-2.87791997799628E-16));
#13380=CARTESIAN_POINT('Origin',(0.,-0.6,0.));
#13381=CARTESIAN_POINT('',(-2.35,0.,-2.87791997799628E-16));
#13382=CARTESIAN_POINT('Origin',(0.,-0.65,0.));
#13383=CARTESIAN_POINT('',(-2.25,-0.7,-2.75545529808154E-16));
#13384=CARTESIAN_POINT('Origin',(0.,-0.7,0.));
#13385=CARTESIAN_POINT('',(-2.3,-0.65,-2.81668763803891E-16));
#13386=CARTESIAN_POINT('Origin',(1.71469,-0.7,0.));
#13387=CARTESIAN_POINT('Origin',(0.,0.,0.));
#13388=CARTESIAN_POINT('',(-1.71469,0.,-2.09988962002998E-16));
#13389=CARTESIAN_POINT('',(0.,0.,0.));
#13390=CARTESIAN_POINT('Origin',(1.675,0.,0.));
#13391=CARTESIAN_POINT('',(1.675,-2.97627328869245E-33,0.3969));
#13392=CARTESIAN_POINT('',(1.675,-2.97627328869245E-33,-0.3969));
#13393=CARTESIAN_POINT('Origin',(1.675,0.,0.));
#13394=CARTESIAN_POINT('Origin',(1.18440385848747,0.,-1.18440385848747));
#13395=CARTESIAN_POINT('',(1.46505453994041,3.1867025333467E-33,-0.903753177034526));
#13396=CARTESIAN_POINT('',(0.903753177034527,-9.13924911073161E-33,-1.46505453994041));
#13397=CARTESIAN_POINT('Origin',(1.18440385848747,0.,-1.18440385848747));
#13398=CARTESIAN_POINT('Origin',(1.02564169428591E-16,0.,-1.675));
#13399=CARTESIAN_POINT('',(0.3969,-2.97627328869246E-33,-1.675));
#13400=CARTESIAN_POINT('',(-0.3969,-2.97627328869245E-33,-1.675));
#13401=CARTESIAN_POINT('Origin',(1.02564169428591E-16,0.,-1.675));
#13402=CARTESIAN_POINT('Origin',(-1.18440385848747,0.,-1.18440385848747));
#13403=CARTESIAN_POINT('',(-0.903753177034526,3.1867025333467E-33,-1.46505453994041));
#13404=CARTESIAN_POINT('',(-1.46505453994041,-9.13924911073161E-33,-0.903753177034527));
#13405=CARTESIAN_POINT('Origin',(-1.18440385848747,0.,-1.18440385848747));
#13406=CARTESIAN_POINT('Origin',(-1.675,0.,-2.05128338857182E-16));
#13407=CARTESIAN_POINT('',(-1.675,-2.97627328869246E-33,-0.3969));
#13408=CARTESIAN_POINT('',(-1.675,-2.97627328869245E-33,0.3969));
#13409=CARTESIAN_POINT('Origin',(-1.675,0.,-2.05128338857182E-16));
#13410=CARTESIAN_POINT('Origin',(-1.18440385848747,0.,1.18440385848747));
#13411=CARTESIAN_POINT('',(-1.46505453994041,6.26819044436628E-33,0.903753177034526));
#13412=CARTESIAN_POINT('',(-0.903753177034527,-1.22207370217512E-32,1.46505453994041));
#13413=CARTESIAN_POINT('Origin',(-1.18440385848747,0.,1.18440385848747));
#13414=CARTESIAN_POINT('Origin',(-3.07692508285772E-16,0.,1.675));
#13415=CARTESIAN_POINT('',(-0.3969,-2.97627328869246E-33,1.675));
#13416=CARTESIAN_POINT('',(0.396899999999999,-2.97627328869245E-33,1.675));
#13417=CARTESIAN_POINT('Origin',(-3.07692508285772E-16,0.,1.675));
#13418=CARTESIAN_POINT('Origin',(1.18440385848747,0.,1.18440385848747));
#13419=CARTESIAN_POINT('',(0.903753177034526,9.34967835538585E-33,1.46505453994041));
#13420=CARTESIAN_POINT('',(1.46505453994041,-1.53022249327708E-32,0.903753177034527));
#13421=CARTESIAN_POINT('Origin',(1.18440385848747,0.,1.18440385848747));
#13422=CARTESIAN_POINT('',(0.,0.,0.));
#13423=CARTESIAN_POINT('Origin',(1.18440385848747,0.,1.18440385848747));
#13424=CARTESIAN_POINT('',(0.846804978391753,-0.07938,1.40825612658882));
#13425=CARTESIAN_POINT('',(1.40825612658882,-0.07938,0.846804978391754));
#13426=CARTESIAN_POINT('Ctrl Pts',(0.846804978391752,-0.0793800000000001,
1.40825612658882));
#13427=CARTESIAN_POINT('Ctrl Pts',(0.854205272175554,-0.123401821157026,
1.40380622184538));
#13428=CARTESIAN_POINT('Ctrl Pts',(0.867957148219441,-0.166543350814306,
1.39550172959303));
#13429=CARTESIAN_POINT('Ctrl Pts',(0.902193646979982,-0.237231147975234,
1.3735491215176));
#13430=CARTESIAN_POINT('Ctrl Pts',(0.920778333482564,-0.266264900654909,
1.36127834356734));
#13431=CARTESIAN_POINT('Ctrl Pts',(0.962485392528369,-0.317195968905306,
1.33211611256184));
#13432=CARTESIAN_POINT('Ctrl Pts',(0.985600426557816,-0.33909093068465,
1.31521005565926));
#13433=CARTESIAN_POINT('Ctrl Pts',(1.03253285680459,-0.373586846396559,
1.27866649102984));
#13434=CARTESIAN_POINT('Ctrl Pts',(1.05871835910697,-0.388086240756494,
1.25722555095714));
#13435=CARTESIAN_POINT('Ctrl Pts',(1.11153475808518,-0.407068917407805,
1.2107812086231));
#13436=CARTESIAN_POINT('Ctrl Pts',(1.13814686046673,-0.411552957311693,
1.18575674747573));
#13437=CARTESIAN_POINT('Ctrl Pts',(1.18575674747573,-0.411552957311693,
1.13814686046673));
#13438=CARTESIAN_POINT('Ctrl Pts',(1.2107812086231,-0.407068917407805,1.11153475808518));
#13439=CARTESIAN_POINT('Ctrl Pts',(1.25722555095713,-0.388086240756494,
1.05871835910697));
#13440=CARTESIAN_POINT('Ctrl Pts',(1.27866649102984,-0.373586846396559,
1.03253285680459));
#13441=CARTESIAN_POINT('Ctrl Pts',(1.31521005565926,-0.33909093068465,0.985600426557816));
#13442=CARTESIAN_POINT('Ctrl Pts',(1.33211611256184,-0.317195968905306,
0.962485392528369));
#13443=CARTESIAN_POINT('Ctrl Pts',(1.36127834356734,-0.266264900654909,
0.920778333482565));
#13444=CARTESIAN_POINT('Ctrl Pts',(1.3735491215176,-0.237231147975234,0.902193646979983));
#13445=CARTESIAN_POINT('Ctrl Pts',(1.39550172959303,-0.166543350814306,
0.867957148219442));
#13446=CARTESIAN_POINT('Ctrl Pts',(1.40380622184538,-0.123401821157026,
0.854205272175555));
#13447=CARTESIAN_POINT('Ctrl Pts',(1.40825612658882,-0.0793800000000001,
0.846804978391753));
#13448=CARTESIAN_POINT('',(0.886256117232623,-0.07938,1.45861320581289));
#13449=CARTESIAN_POINT('Origin',(1.18440385848747,-0.07938,1.18440385848747));
#13450=CARTESIAN_POINT('',(1.45861320581289,-0.07938,0.886256117232624));
#13451=CARTESIAN_POINT('Ctrl Pts',(1.45861320581289,-0.0793800000000001,
0.886256117232623));
#13452=CARTESIAN_POINT('Ctrl Pts',(1.45630208793976,-0.101649918886749,
0.890059788636852));
#13453=CARTESIAN_POINT('Ctrl Pts',(1.45296717977858,-0.123823518623746,
0.895520212222107));
#13454=CARTESIAN_POINT('Ctrl Pts',(1.43904931717599,-0.192480977588836,
0.917859913453975));
#13455=CARTESIAN_POINT('Ctrl Pts',(1.4243271592157,-0.236152929235938,0.940896403863072));
#13456=CARTESIAN_POINT('Ctrl Pts',(1.39055359345152,-0.303141259068212,
0.990027513266106));
#13457=CARTESIAN_POINT('Ctrl Pts',(1.36743459453896,-0.335108247315849,
1.02199477007745));
#13458=CARTESIAN_POINT('Ctrl Pts',(1.32643091652006,-0.373243761060364,
1.07446535104584));
#13459=CARTESIAN_POINT('Ctrl Pts',(1.30441816675528,-0.387888272594439,
1.10126842659597));
#13460=CARTESIAN_POINT('Ctrl Pts',(1.25681160160691,-0.407041111792943,
1.15530234155453));
#13461=CARTESIAN_POINT('Ctrl Pts',(1.23119764287622,-0.411552957311693,
1.18251418313119));
#13462=CARTESIAN_POINT('Ctrl Pts',(1.18251418313119,-0.411552957311693,
1.23119764287622));
#13463=CARTESIAN_POINT('Ctrl Pts',(1.15530234155453,-0.407041111792943,
1.25681160160691));
#13464=CARTESIAN_POINT('Ctrl Pts',(1.10126842659597,-0.387888272594439,
1.30441816675528));
#13465=CARTESIAN_POINT('Ctrl Pts',(1.07446535104584,-0.373243761060364,
1.32643091652006));
#13466=CARTESIAN_POINT('Ctrl Pts',(1.02199477007745,-0.335108247315848,
1.36743459453896));
#13467=CARTESIAN_POINT('Ctrl Pts',(0.990027513266105,-0.303141259068211,
1.39055359345152));
#13468=CARTESIAN_POINT('Ctrl Pts',(0.940896403863071,-0.236152929235937,
1.42432715921571));
#13469=CARTESIAN_POINT('Ctrl Pts',(0.917859913453974,-0.192480977588835,
1.43904931717599));
#13470=CARTESIAN_POINT('Ctrl Pts',(0.895520212222106,-0.123823518623745,
1.45296717977858));
#13471=CARTESIAN_POINT('Ctrl Pts',(0.890059788636851,-0.101649918886749,
1.45630208793976));
#13472=CARTESIAN_POINT('Ctrl Pts',(0.886256117232622,-0.0793800000000001,
1.45861320581289));
#13473=CARTESIAN_POINT('Origin',(1.18440385848747,-0.07938,1.18440385848747));
#13474=CARTESIAN_POINT('Origin',(0.,-0.27783,0.));
#13475=CARTESIAN_POINT('',(0.404717578595295,-0.07938,1.65807299932179));
#13476=CARTESIAN_POINT('Origin',(0.,-0.07938,0.));
#13477=CARTESIAN_POINT('',(-0.404717578595296,-0.07938,1.65807299932179));
#13478=CARTESIAN_POINT('Ctrl Pts',(0.404717578595296,-0.0793800000000001,
1.65807299932179));
#13479=CARTESIAN_POINT('Ctrl Pts',(0.400393769631747,-0.101649918886749,
1.65912839404491));
#13480=CARTESIAN_POINT('Ctrl Pts',(0.394174530911058,-0.123823518623745,
1.66063136041479));
#13481=CARTESIAN_POINT('Ctrl Pts',(0.368536561654407,-0.192480977588835,
1.66658649961961));
#13482=CARTESIAN_POINT('Ctrl Pts',(0.341837165343982,-0.236152929235937,
1.67246562047521));
#13483=CARTESIAN_POINT('Ctrl Pts',(0.283214707341173,-0.303141259068211,
1.68332504372461));
#13484=CARTESIAN_POINT('Ctrl Pts',(0.244262842368623,-0.335108247315849,
1.68958170688653));
#13485=CARTESIAN_POINT('Ctrl Pts',(0.178166559972324,-0.373243761060364,
1.69769003172132));
#13486=CARTESIAN_POINT('Ctrl Pts',(0.143648558862931,-0.387888272594439,
1.70107730356824));
#13487=CARTESIAN_POINT('Ctrl Pts',(0.0717778861362652,-0.407041111792943,
1.70562212620408));
#13488=CARTESIAN_POINT('Ctrl Pts',(0.0344244045173309,-0.411552957311693,
1.706752));
#13489=CARTESIAN_POINT('Ctrl Pts',(-0.0344244045173315,-0.411552957311693,
1.706752));
#13490=CARTESIAN_POINT('Ctrl Pts',(-0.0717778861362658,-0.407041111792943,
1.70562212620408));
#13491=CARTESIAN_POINT('Ctrl Pts',(-0.143648558862932,-0.387888272594439,
1.70107730356824));
#13492=CARTESIAN_POINT('Ctrl Pts',(-0.178166559972325,-0.373243761060364,
1.69769003172132));
#13493=CARTESIAN_POINT('Ctrl Pts',(-0.244262842368624,-0.335108247315849,
1.68958170688653));
#13494=CARTESIAN_POINT('Ctrl Pts',(-0.283214707341173,-0.303141259068212,
1.68332504372461));
#13495=CARTESIAN_POINT('Ctrl Pts',(-0.341837165343982,-0.236152929235937,
1.67246562047521));
#13496=CARTESIAN_POINT('Ctrl Pts',(-0.368536561654408,-0.192480977588835,
1.66658649961961));
#13497=CARTESIAN_POINT('Ctrl Pts',(-0.394174530911059,-0.123823518623745,
1.66063136041479));
#13498=CARTESIAN_POINT('Ctrl Pts',(-0.400393769631748,-0.101649918886749,
1.65912839404491));
#13499=CARTESIAN_POINT('Ctrl Pts',(-0.404717578595297,-0.0793800000000001,
1.65807299932179));
#13500=CARTESIAN_POINT('',(-0.886256117232624,-0.07938,1.45861320581289));
#13501=CARTESIAN_POINT('Origin',(0.,-0.07938,0.));
#13502=CARTESIAN_POINT('',(-1.45861320581289,-0.07938,0.886256117232623));
#13503=CARTESIAN_POINT('Ctrl Pts',(-0.886256117232623,-0.0793800000000001,
1.45861320581289));
#13504=CARTESIAN_POINT('Ctrl Pts',(-0.890059788636852,-0.101649918886749,
1.45630208793976));
#13505=CARTESIAN_POINT('Ctrl Pts',(-0.895520212222106,-0.123823518623745,
1.45296717977858));
#13506=CARTESIAN_POINT('Ctrl Pts',(-0.917859913453974,-0.192480977588835,
1.43904931717599));
#13507=CARTESIAN_POINT('Ctrl Pts',(-0.940896403863071,-0.236152929235937,
1.4243271592157));
#13508=CARTESIAN_POINT('Ctrl Pts',(-0.990027513266105,-0.303141259068211,
1.39055359345152));
#13509=CARTESIAN_POINT('Ctrl Pts',(-1.02199477007745,-0.335108247315848,
1.36743459453896));
#13510=CARTESIAN_POINT('Ctrl Pts',(-1.07446535104584,-0.373243761060364,
1.32643091652006));
#13511=CARTESIAN_POINT('Ctrl Pts',(-1.10126842659597,-0.387888272594439,
1.30441816675528));
#13512=CARTESIAN_POINT('Ctrl Pts',(-1.15530234155453,-0.407041111792943,
1.25681160160691));
#13513=CARTESIAN_POINT('Ctrl Pts',(-1.18251418313119,-0.411552957311693,
1.23119764287622));
#13514=CARTESIAN_POINT('Ctrl Pts',(-1.23119764287622,-0.411552957311693,
1.18251418313119));
#13515=CARTESIAN_POINT('Ctrl Pts',(-1.25681160160691,-0.407041111792943,
1.15530234155453));
#13516=CARTESIAN_POINT('Ctrl Pts',(-1.30441816675528,-0.387888272594439,
1.10126842659597));
#13517=CARTESIAN_POINT('Ctrl Pts',(-1.32643091652006,-0.373243761060365,
1.07446535104584));
#13518=CARTESIAN_POINT('Ctrl Pts',(-1.36743459453896,-0.335108247315849,
1.02199477007745));
#13519=CARTESIAN_POINT('Ctrl Pts',(-1.39055359345152,-0.303141259068212,
0.990027513266106));
#13520=CARTESIAN_POINT('Ctrl Pts',(-1.4243271592157,-0.236152929235938,
0.940896403863071));
#13521=CARTESIAN_POINT('Ctrl Pts',(-1.43904931717599,-0.192480977588836,
0.917859913453974));
#13522=CARTESIAN_POINT('Ctrl Pts',(-1.45296717977858,-0.123823518623746,
0.895520212222106));
#13523=CARTESIAN_POINT('Ctrl Pts',(-1.45630208793976,-0.101649918886749,
0.890059788636852));
#13524=CARTESIAN_POINT('Ctrl Pts',(-1.45861320581289,-0.0793800000000001,
0.886256117232623));
#13525=CARTESIAN_POINT('',(-1.65807299932179,-0.07938,0.404717578595295));
#13526=CARTESIAN_POINT('Origin',(0.,-0.07938,0.));
#13527=CARTESIAN_POINT('',(-1.706752,-0.411552957311693,2.08591827245526E-16));
#13528=CARTESIAN_POINT('Ctrl Pts',(-1.65807299932179,-0.0793800000000001,
0.404717578595296));
#13529=CARTESIAN_POINT('Ctrl Pts',(-1.65912839404491,-0.101649918886749,
0.400393769631747));
#13530=CARTESIAN_POINT('Ctrl Pts',(-1.66063136041479,-0.123823518623745,
0.394174530911058));
#13531=CARTESIAN_POINT('Ctrl Pts',(-1.66658649961961,-0.192480977588835,
0.368536561654407));
#13532=CARTESIAN_POINT('Ctrl Pts',(-1.67246562047521,-0.236152929235937,
0.341837165343982));
#13533=CARTESIAN_POINT('Ctrl Pts',(-1.68332504372461,-0.303141259068211,
0.283214707341173));
#13534=CARTESIAN_POINT('Ctrl Pts',(-1.68958170688653,-0.335108247315848,
0.244262842368623));
#13535=CARTESIAN_POINT('Ctrl Pts',(-1.69769003172132,-0.373243761060364,
0.178166559972324));
#13536=CARTESIAN_POINT('Ctrl Pts',(-1.70107730356824,-0.387888272594439,
0.143648558862931));
#13537=CARTESIAN_POINT('Ctrl Pts',(-1.70562212620408,-0.407041111792943,
0.0717778861362656));
#13538=CARTESIAN_POINT('Ctrl Pts',(-1.706752,-0.411552957311693,0.0344244045173313));
#13539=CARTESIAN_POINT('Ctrl Pts',(-1.706752,-0.411552957311693,2.08166817117217E-16));
#13540=CARTESIAN_POINT('',(-1.706752,-0.47628,2.09016837373834E-16));
#13541=CARTESIAN_POINT('',(-1.706752,-0.27783,2.09016837373834E-16));
#13542=CARTESIAN_POINT('Origin',(0.,-0.47628,0.));
#13543=CARTESIAN_POINT('',(-1.65807299932179,-0.07938,-0.404717578595296));
#13544=CARTESIAN_POINT('Ctrl Pts',(-1.706752,-0.411552957311693,2.0122792321331E-16));
#13545=CARTESIAN_POINT('Ctrl Pts',(-1.706752,-0.411552957311693,-0.0344244045173309));
#13546=CARTESIAN_POINT('Ctrl Pts',(-1.70562212620408,-0.407041111792943,
-0.0717778861362652));
#13547=CARTESIAN_POINT('Ctrl Pts',(-1.70107730356824,-0.387888272594439,
-0.143648558862931));
#13548=CARTESIAN_POINT('Ctrl Pts',(-1.69769003172132,-0.373243761060365,
-0.178166559972324));
#13549=CARTESIAN_POINT('Ctrl Pts',(-1.68958170688653,-0.335108247315849,
-0.244262842368623));
#13550=CARTESIAN_POINT('Ctrl Pts',(-1.68332504372461,-0.303141259068212,
-0.283214707341173));
#13551=CARTESIAN_POINT('Ctrl Pts',(-1.67246562047521,-0.236152929235938,
-0.341837165343982));
#13552=CARTESIAN_POINT('Ctrl Pts',(-1.66658649961961,-0.192480977588836,
-0.368536561654407));
#13553=CARTESIAN_POINT('Ctrl Pts',(-1.66063136041479,-0.123823518623745,
-0.394174530911059));
#13554=CARTESIAN_POINT('Ctrl Pts',(-1.65912839404491,-0.101649918886749,
-0.400393769631748));
#13555=CARTESIAN_POINT('Ctrl Pts',(-1.65807299932179,-0.0793800000000001,
-0.404717578595296));
#13556=CARTESIAN_POINT('',(-1.45861320581289,-0.07938,-0.886256117232623));
#13557=CARTESIAN_POINT('Origin',(0.,-0.07938,0.));
#13558=CARTESIAN_POINT('',(-0.886256117232623,-0.07938,-1.45861320581289));
#13559=CARTESIAN_POINT('Ctrl Pts',(-1.45861320581289,-0.0793800000000001,
-0.886256117232623));
#13560=CARTESIAN_POINT('Ctrl Pts',(-1.45630208793976,-0.101649918886749,
-0.890059788636852));
#13561=CARTESIAN_POINT('Ctrl Pts',(-1.45296717977858,-0.123823518623745,
-0.895520212222106));
#13562=CARTESIAN_POINT('Ctrl Pts',(-1.43904931717599,-0.192480977588835,
-0.917859913453974));
#13563=CARTESIAN_POINT('Ctrl Pts',(-1.4243271592157,-0.236152929235937,
-0.940896403863072));
#13564=CARTESIAN_POINT('Ctrl Pts',(-1.39055359345152,-0.303141259068212,
-0.990027513266106));
#13565=CARTESIAN_POINT('Ctrl Pts',(-1.36743459453896,-0.335108247315849,
-1.02199477007745));
#13566=CARTESIAN_POINT('Ctrl Pts',(-1.32643091652006,-0.373243761060364,
-1.07446535104584));
#13567=CARTESIAN_POINT('Ctrl Pts',(-1.30441816675528,-0.387888272594439,
-1.10126842659597));
#13568=CARTESIAN_POINT('Ctrl Pts',(-1.25681160160691,-0.407041111792943,
-1.15530234155453));
#13569=CARTESIAN_POINT('Ctrl Pts',(-1.23119764287622,-0.411552957311693,
-1.18251418313119));
#13570=CARTESIAN_POINT('Ctrl Pts',(-1.18251418313119,-0.411552957311693,
-1.23119764287622));
#13571=CARTESIAN_POINT('Ctrl Pts',(-1.15530234155453,-0.407041111792943,
-1.25681160160691));
#13572=CARTESIAN_POINT('Ctrl Pts',(-1.10126842659597,-0.387888272594439,
-1.30441816675528));
#13573=CARTESIAN_POINT('Ctrl Pts',(-1.07446535104584,-0.373243761060364,
-1.32643091652006));
#13574=CARTESIAN_POINT('Ctrl Pts',(-1.02199477007745,-0.335108247315848,
-1.36743459453896));
#13575=CARTESIAN_POINT('Ctrl Pts',(-0.990027513266105,-0.303141259068211,
-1.39055359345152));
#13576=CARTESIAN_POINT('Ctrl Pts',(-0.940896403863071,-0.236152929235936,
-1.42432715921571));
#13577=CARTESIAN_POINT('Ctrl Pts',(-0.917859913453974,-0.192480977588835,
-1.43904931717599));
#13578=CARTESIAN_POINT('Ctrl Pts',(-0.895520212222106,-0.123823518623745,
-1.45296717977858));
#13579=CARTESIAN_POINT('Ctrl Pts',(-0.890059788636851,-0.101649918886749,
-1.45630208793976));
#13580=CARTESIAN_POINT('Ctrl Pts',(-0.886256117232623,-0.0793800000000001,
-1.45861320581289));
#13581=CARTESIAN_POINT('',(-0.404717578595295,-0.07938,-1.65807299932179));
#13582=CARTESIAN_POINT('Origin',(0.,-0.07938,0.));
#13583=CARTESIAN_POINT('',(0.404717578595296,-0.07938,-1.65807299932179));
#13584=CARTESIAN_POINT('Ctrl Pts',(-0.404717578595296,-0.0793800000000001,
-1.65807299932179));
#13585=CARTESIAN_POINT('Ctrl Pts',(-0.400393769631747,-0.101649918886749,
-1.65912839404491));
#13586=CARTESIAN_POINT('Ctrl Pts',(-0.394174530911058,-0.123823518623746,
-1.66063136041479));
#13587=CARTESIAN_POINT('Ctrl Pts',(-0.368536561654407,-0.192480977588836,
-1.66658649961961));
#13588=CARTESIAN_POINT('Ctrl Pts',(-0.341837165343982,-0.236152929235938,
-1.67246562047521));
#13589=CARTESIAN_POINT('Ctrl Pts',(-0.283214707341173,-0.303141259068212,
-1.68332504372461));
#13590=CARTESIAN_POINT('Ctrl Pts',(-0.244262842368623,-0.335108247315849,
-1.68958170688653));
#13591=CARTESIAN_POINT('Ctrl Pts',(-0.178166559972324,-0.373243761060364,
-1.69769003172132));
#13592=CARTESIAN_POINT('Ctrl Pts',(-0.143648558862931,-0.387888272594439,
-1.70107730356824));
#13593=CARTESIAN_POINT('Ctrl Pts',(-0.0717778861362653,-0.407041111792943,
-1.70562212620408));
#13594=CARTESIAN_POINT('Ctrl Pts',(-0.034424404517331,-0.411552957311693,
-1.706752));
#13595=CARTESIAN_POINT('Ctrl Pts',(0.0344244045173312,-0.411552957311693,
-1.706752));
#13596=CARTESIAN_POINT('Ctrl Pts',(0.0717778861362655,-0.407041111792943,
-1.70562212620408));
#13597=CARTESIAN_POINT('Ctrl Pts',(0.143648558862931,-0.387888272594439,
-1.70107730356824));
#13598=CARTESIAN_POINT('Ctrl Pts',(0.178166559972324,-0.373243761060364,
-1.69769003172132));
#13599=CARTESIAN_POINT('Ctrl Pts',(0.244262842368623,-0.335108247315849,
-1.68958170688653));
#13600=CARTESIAN_POINT('Ctrl Pts',(0.283214707341173,-0.303141259068212,
-1.68332504372461));
#13601=CARTESIAN_POINT('Ctrl Pts',(0.341837165343982,-0.236152929235937,
-1.67246562047521));
#13602=CARTESIAN_POINT('Ctrl Pts',(0.368536561654407,-0.192480977588835,
-1.66658649961961));
#13603=CARTESIAN_POINT('Ctrl Pts',(0.394174530911059,-0.123823518623745,
-1.66063136041479));
#13604=CARTESIAN_POINT('Ctrl Pts',(0.400393769631748,-0.101649918886749,
-1.65912839404491));
#13605=CARTESIAN_POINT('Ctrl Pts',(0.404717578595296,-0.0793800000000001,
-1.65807299932179));
#13606=CARTESIAN_POINT('',(0.886256117232623,-0.07938,-1.45861320581289));
#13607=CARTESIAN_POINT('Origin',(0.,-0.07938,0.));
#13608=CARTESIAN_POINT('',(1.45861320581289,-0.07938,-0.886256117232623));
#13609=CARTESIAN_POINT('Ctrl Pts',(0.886256117232623,-0.0793800000000001,
-1.45861320581289));
#13610=CARTESIAN_POINT('Ctrl Pts',(0.890059788636852,-0.101649918886749,
-1.45630208793976));
#13611=CARTESIAN_POINT('Ctrl Pts',(0.895520212222106,-0.123823518623745,
-1.45296717977858));
#13612=CARTESIAN_POINT('Ctrl Pts',(0.917859913453974,-0.192480977588835,
-1.43904931717599));
#13613=CARTESIAN_POINT('Ctrl Pts',(0.940896403863072,-0.236152929235937,
-1.4243271592157));
#13614=CARTESIAN_POINT('Ctrl Pts',(0.990027513266106,-0.303141259068211,
-1.39055359345152));
#13615=CARTESIAN_POINT('Ctrl Pts',(1.02199477007745,-0.335108247315849,
-1.36743459453896));
#13616=CARTESIAN_POINT('Ctrl Pts',(1.07446535104584,-0.373243761060364,
-1.32643091652006));
#13617=CARTESIAN_POINT('Ctrl Pts',(1.10126842659597,-0.387888272594439,
-1.30441816675528));
#13618=CARTESIAN_POINT('Ctrl Pts',(1.15530234155453,-0.407041111792943,
-1.25681160160691));
#13619=CARTESIAN_POINT('Ctrl Pts',(1.18251418313119,-0.411552957311693,
-1.23119764287622));
#13620=CARTESIAN_POINT('Ctrl Pts',(1.23119764287622,-0.411552957311693,
-1.18251418313119));
#13621=CARTESIAN_POINT('Ctrl Pts',(1.25681160160691,-0.407041111792943,
-1.15530234155453));
#13622=CARTESIAN_POINT('Ctrl Pts',(1.30441816675528,-0.387888272594439,
-1.10126842659597));
#13623=CARTESIAN_POINT('Ctrl Pts',(1.32643091652006,-0.373243761060364,
-1.07446535104584));
#13624=CARTESIAN_POINT('Ctrl Pts',(1.36743459453896,-0.335108247315849,
-1.02199477007745));
#13625=CARTESIAN_POINT('Ctrl Pts',(1.39055359345152,-0.303141259068212,
-0.990027513266105));
#13626=CARTESIAN_POINT('Ctrl Pts',(1.4243271592157,-0.236152929235937,-0.940896403863071));
#13627=CARTESIAN_POINT('Ctrl Pts',(1.43904931717599,-0.192480977588835,
-0.917859913453974));
#13628=CARTESIAN_POINT('Ctrl Pts',(1.45296717977858,-0.123823518623745,
-0.895520212222106));
#13629=CARTESIAN_POINT('Ctrl Pts',(1.45630208793976,-0.101649918886749,
-0.890059788636852));
#13630=CARTESIAN_POINT('Ctrl Pts',(1.45861320581289,-0.0793800000000001,
-0.886256117232623));
#13631=CARTESIAN_POINT('',(1.65807299932179,-0.07938,-0.404717578595296));
#13632=CARTESIAN_POINT('Origin',(0.,-0.07938,0.));
#13633=CARTESIAN_POINT('',(1.65807299932179,-0.07938,0.404717578595296));
#13634=CARTESIAN_POINT('Ctrl Pts',(1.65807299932179,-0.0793800000000001,
-0.404717578595296));
#13635=CARTESIAN_POINT('Ctrl Pts',(1.65912839404491,-0.101649918886749,
-0.400393769631747));
#13636=CARTESIAN_POINT('Ctrl Pts',(1.66063136041479,-0.123823518623745,
-0.394174530911058));
#13637=CARTESIAN_POINT('Ctrl Pts',(1.66658649961961,-0.192480977588835,
-0.368536561654407));
#13638=CARTESIAN_POINT('Ctrl Pts',(1.67246562047521,-0.236152929235937,
-0.341837165343982));
#13639=CARTESIAN_POINT('Ctrl Pts',(1.68332504372461,-0.303141259068212,
-0.283214707341173));
#13640=CARTESIAN_POINT('Ctrl Pts',(1.68958170688653,-0.335108247315849,
-0.244262842368623));
#13641=CARTESIAN_POINT('Ctrl Pts',(1.69769003172132,-0.373243761060364,
-0.178166559972324));
#13642=CARTESIAN_POINT('Ctrl Pts',(1.70107730356824,-0.387888272594439,
-0.143648558862931));
#13643=CARTESIAN_POINT('Ctrl Pts',(1.70562212620408,-0.407041111792943,
-0.0717778861362655));
#13644=CARTESIAN_POINT('Ctrl Pts',(1.706752,-0.411552957311693,-0.0344244045173312));
#13645=CARTESIAN_POINT('Ctrl Pts',(1.706752,-0.411552957311693,0.0344244045173312));
#13646=CARTESIAN_POINT('Ctrl Pts',(1.70562212620408,-0.407041111792943,
0.0717778861362655));
#13647=CARTESIAN_POINT('Ctrl Pts',(1.70107730356824,-0.387888272594439,
0.143648558862931));
#13648=CARTESIAN_POINT('Ctrl Pts',(1.69769003172132,-0.373243761060364,
0.178166559972324));
#13649=CARTESIAN_POINT('Ctrl Pts',(1.68958170688653,-0.335108247315849,
0.244262842368623));
#13650=CARTESIAN_POINT('Ctrl Pts',(1.68332504372461,-0.303141259068212,
0.283214707341173));
#13651=CARTESIAN_POINT('Ctrl Pts',(1.67246562047521,-0.236152929235937,
0.341837165343982));
#13652=CARTESIAN_POINT('Ctrl Pts',(1.66658649961961,-0.192480977588835,
0.368536561654407));
#13653=CARTESIAN_POINT('Ctrl Pts',(1.66063136041479,-0.123823518623745,
0.394174530911058));
#13654=CARTESIAN_POINT('Ctrl Pts',(1.65912839404491,-0.101649918886749,
0.400393769631747));
#13655=CARTESIAN_POINT('Ctrl Pts',(1.65807299932179,-0.0793800000000001,
0.404717578595296));
#13656=CARTESIAN_POINT('Origin',(0.,-0.07938,0.));
#13657=CARTESIAN_POINT('Origin',(0.,-0.07938,0.));
#13658=CARTESIAN_POINT('',(0.397005914195118,-0.07938,1.59456899932179));
#13659=CARTESIAN_POINT('Origin',(0.,-0.07938,0.));
#13660=CARTESIAN_POINT('Origin',(-3.33066907387547E-16,-0.07938,1.675));
#13661=CARTESIAN_POINT('Origin',(-3.33066907387547E-16,0.,1.675));
#13662=CARTESIAN_POINT('',(-0.397005914195118,-0.07938,1.59456899932179));
#13663=CARTESIAN_POINT('Ctrl Pts',(-0.397005914195119,-0.0793800000000001,
1.59456899932179));
#13664=CARTESIAN_POINT('Ctrl Pts',(-0.3886265584581,-0.123401821157026,
1.59665523941937));
#13665=CARTESIAN_POINT('Ctrl Pts',(-0.373030350867485,-0.166543350814306,
1.60050712143809));
#13666=CARTESIAN_POINT('Ctrl Pts',(-0.333298652394954,-0.237231147975234,
1.60919314384089));
#13667=CARTESIAN_POINT('Ctrl Pts',(-0.311480544243687,-0.266264900654909,
1.61365775139403));
#13668=CARTESIAN_POINT('Ctrl Pts',(-0.261368388670537,-0.317195968905306,
1.62252828437015));
#13669=CARTESIAN_POINT('Ctrl Pts',(-0.233069203882014,-0.33909093068465,
1.62691869420078));
#13670=CARTESIAN_POINT('Ctrl Pts',(-0.174042761838764,-0.373586846396559,
1.63426473152765));
#13671=CARTESIAN_POINT('Ctrl Pts',(-0.14036578147155,-0.388086240756494,
1.63761964365402));
#13672=CARTESIAN_POINT('Ctrl Pts',(-0.0701778381840615,-0.407068917407805,
1.64212536811722));
#13673=CARTESIAN_POINT('Ctrl Pts',(-0.0336652739555918,-0.411552957311693,
1.643248));
#13674=CARTESIAN_POINT('Ctrl Pts',(0.0336652739555913,-0.411552957311693,
1.643248));
#13675=CARTESIAN_POINT('Ctrl Pts',(0.070177838184061,-0.407068917407805,
1.64212536811722));
#13676=CARTESIAN_POINT('Ctrl Pts',(0.140365781471549,-0.388086240756494,
1.63761964365402));
#13677=CARTESIAN_POINT('Ctrl Pts',(0.174042761838763,-0.373586846396559,
1.63426473152765));
#13678=CARTESIAN_POINT('Ctrl Pts',(0.233069203882014,-0.33909093068465,
1.62691869420078));
#13679=CARTESIAN_POINT('Ctrl Pts',(0.261368388670536,-0.317195968905306,
1.62252828437015));
#13680=CARTESIAN_POINT('Ctrl Pts',(0.311480544243686,-0.266264900654908,
1.61365775139403));
#13681=CARTESIAN_POINT('Ctrl Pts',(0.333298652394954,-0.237231147975234,
1.60919314384089));
#13682=CARTESIAN_POINT('Ctrl Pts',(0.373030350867484,-0.166543350814306,
1.60050712143809));
#13683=CARTESIAN_POINT('Ctrl Pts',(0.388626558458099,-0.123401821157026,
1.59665523941937));
#13684=CARTESIAN_POINT('Ctrl Pts',(0.397005914195118,-0.07938,1.59456899932179));
#13685=CARTESIAN_POINT('Origin',(-3.33066907387547E-16,-0.07938,1.675));
#13686=CARTESIAN_POINT('Origin',(0.,-0.07938,0.));
#13687=CARTESIAN_POINT('',(-0.846804978391754,-0.07938,1.40825612658882));
#13688=CARTESIAN_POINT('Origin',(0.,-0.07938,0.));
#13689=CARTESIAN_POINT('Origin',(-1.18440385848747,-0.07938,1.18440385848747));
#13690=CARTESIAN_POINT('Origin',(-1.18440385848747,0.,1.18440385848747));
#13691=CARTESIAN_POINT('',(-1.40825612658882,-0.07938,0.846804978391753));
#13692=CARTESIAN_POINT('Ctrl Pts',(-1.40825612658882,-0.0793800000000001,
0.846804978391753));
#13693=CARTESIAN_POINT('Ctrl Pts',(-1.40380622184538,-0.123401821157026,
0.854205272175555));
#13694=CARTESIAN_POINT('Ctrl Pts',(-1.39550172959303,-0.166543350814306,
0.867957148219442));
#13695=CARTESIAN_POINT('Ctrl Pts',(-1.3735491215176,-0.237231147975235,
0.902193646979983));
#13696=CARTESIAN_POINT('Ctrl Pts',(-1.36127834356734,-0.266264900654909,
0.920778333482565));
#13697=CARTESIAN_POINT('Ctrl Pts',(-1.33211611256184,-0.317195968905306,
0.962485392528369));
#13698=CARTESIAN_POINT('Ctrl Pts',(-1.31521005565926,-0.339090930684651,
0.985600426557816));
#13699=CARTESIAN_POINT('Ctrl Pts',(-1.27866649102984,-0.373586846396559,
1.03253285680459));
#13700=CARTESIAN_POINT('Ctrl Pts',(-1.25722555095714,-0.388086240756494,
1.05871835910697));
#13701=CARTESIAN_POINT('Ctrl Pts',(-1.2107812086231,-0.407068917407805,
1.11153475808518));
#13702=CARTESIAN_POINT('Ctrl Pts',(-1.18575674747573,-0.411552957311693,
1.13814686046673));
#13703=CARTESIAN_POINT('Ctrl Pts',(-1.13814686046673,-0.411552957311693,
1.18575674747573));
#13704=CARTESIAN_POINT('Ctrl Pts',(-1.11153475808518,-0.407068917407805,
1.2107812086231));
#13705=CARTESIAN_POINT('Ctrl Pts',(-1.05871835910697,-0.388086240756494,
1.25722555095714));
#13706=CARTESIAN_POINT('Ctrl Pts',(-1.03253285680459,-0.373586846396559,
1.27866649102984));
#13707=CARTESIAN_POINT('Ctrl Pts',(-0.985600426557816,-0.33909093068465,
1.31521005565926));
#13708=CARTESIAN_POINT('Ctrl Pts',(-0.962485392528369,-0.317195968905306,
1.33211611256184));
#13709=CARTESIAN_POINT('Ctrl Pts',(-0.920778333482565,-0.266264900654908,
1.36127834356734));
#13710=CARTESIAN_POINT('Ctrl Pts',(-0.902193646979983,-0.237231147975234,
1.3735491215176));
#13711=CARTESIAN_POINT('Ctrl Pts',(-0.867957148219442,-0.166543350814306,
1.39550172959303));
#13712=CARTESIAN_POINT('Ctrl Pts',(-0.854205272175555,-0.123401821157026,
1.40380622184538));
#13713=CARTESIAN_POINT('Ctrl Pts',(-0.846804978391753,-0.0793800000000001,
1.40825612658882));
#13714=CARTESIAN_POINT('Origin',(-1.18440385848747,-0.07938,1.18440385848747));
#13715=CARTESIAN_POINT('Origin',(0.,-0.07938,0.));
#13716=CARTESIAN_POINT('',(-1.59456899932179,-0.07938,0.397005914195118));
#13717=CARTESIAN_POINT('Origin',(0.,-0.07938,0.));
#13718=CARTESIAN_POINT('Origin',(-1.675,-0.07938,-2.22044604925031E-16));
#13719=CARTESIAN_POINT('Origin',(-1.675,0.,-2.22044604925031E-16));
#13720=CARTESIAN_POINT('',(-1.59456899932179,-0.07938,-0.397005914195118));
#13721=CARTESIAN_POINT('',(-1.643248,-0.411552957311693,3.47540551556327E-18));
#13722=CARTESIAN_POINT('Ctrl Pts',(-1.59456899932179,-0.0793800000000001,
-0.397005914195119));
#13723=CARTESIAN_POINT('Ctrl Pts',(-1.59665523941937,-0.123401821157026,
-0.388626558458099));
#13724=CARTESIAN_POINT('Ctrl Pts',(-1.60050712143809,-0.166543350814306,
-0.373030350867485));
#13725=CARTESIAN_POINT('Ctrl Pts',(-1.60919314384089,-0.237231147975234,
-0.333298652394954));
#13726=CARTESIAN_POINT('Ctrl Pts',(-1.61365775139403,-0.266264900654909,
-0.311480544243686));
#13727=CARTESIAN_POINT('Ctrl Pts',(-1.62252828437015,-0.317195968905306,
-0.261368388670537));
#13728=CARTESIAN_POINT('Ctrl Pts',(-1.62691869420078,-0.33909093068465,
-0.233069203882014));
#13729=CARTESIAN_POINT('Ctrl Pts',(-1.63426473152765,-0.373586846396559,
-0.174042761838764));
#13730=CARTESIAN_POINT('Ctrl Pts',(-1.63761964365402,-0.388086240756494,
-0.140365781471549));
#13731=CARTESIAN_POINT('Ctrl Pts',(-1.64212536811722,-0.407068917407805,
-0.0701778381840614));
#13732=CARTESIAN_POINT('Ctrl Pts',(-1.643248,-0.411552957311693,-0.0336652739555917));
#13733=CARTESIAN_POINT('Ctrl Pts',(-1.643248,-0.411552957311693,-2.0122792321331E-16));
#13734=CARTESIAN_POINT('Origin',(-1.675,-0.07938,-2.22044604925031E-16));
#13735=CARTESIAN_POINT('Ctrl Pts',(-1.643248,-0.411552957311693,-1.94289029309402E-16));
#13736=CARTESIAN_POINT('Ctrl Pts',(-1.643248,-0.411552957311693,0.0336652739555913));
#13737=CARTESIAN_POINT('Ctrl Pts',(-1.64212536811722,-0.407068917407805,
0.0701778381840609));
#13738=CARTESIAN_POINT('Ctrl Pts',(-1.63761964365402,-0.388086240756494,
0.140365781471549));
#13739=CARTESIAN_POINT('Ctrl Pts',(-1.63426473152765,-0.373586846396559,
0.174042761838763));
#13740=CARTESIAN_POINT('Ctrl Pts',(-1.62691869420078,-0.33909093068465,
0.233069203882014));
#13741=CARTESIAN_POINT('Ctrl Pts',(-1.62252828437015,-0.317195968905306,
0.261368388670536));
#13742=CARTESIAN_POINT('Ctrl Pts',(-1.61365775139403,-0.266264900654909,
0.311480544243686));
#13743=CARTESIAN_POINT('Ctrl Pts',(-1.60919314384089,-0.237231147975235,
0.333298652394954));
#13744=CARTESIAN_POINT('Ctrl Pts',(-1.60050712143809,-0.166543350814306,
0.373030350867484));
#13745=CARTESIAN_POINT('Ctrl Pts',(-1.59665523941937,-0.123401821157026,
0.388626558458099));
#13746=CARTESIAN_POINT('Ctrl Pts',(-1.59456899932179,-0.0793800000000001,
0.397005914195118));
#13747=CARTESIAN_POINT('Origin',(0.,-0.07938,0.));
#13748=CARTESIAN_POINT('',(-1.40825612658882,-0.07938,-0.846804978391753));
#13749=CARTESIAN_POINT('Origin',(0.,-0.07938,0.));
#13750=CARTESIAN_POINT('Origin',(-1.18440385848747,-0.07938,-1.18440385848747));
#13751=CARTESIAN_POINT('Origin',(-1.18440385848747,0.,-1.18440385848747));
#13752=CARTESIAN_POINT('',(-0.846804978391753,-0.07938,-1.40825612658882));
#13753=CARTESIAN_POINT('Ctrl Pts',(-0.846804978391753,-0.0793800000000001,
-1.40825612658882));
#13754=CARTESIAN_POINT('Ctrl Pts',(-0.854205272175555,-0.123401821157026,
-1.40380622184538));
#13755=CARTESIAN_POINT('Ctrl Pts',(-0.867957148219442,-0.166543350814306,
-1.39550172959303));
#13756=CARTESIAN_POINT('Ctrl Pts',(-0.902193646979982,-0.237231147975234,
-1.3735491215176));
#13757=CARTESIAN_POINT('Ctrl Pts',(-0.920778333482564,-0.266264900654908,
-1.36127834356734));
#13758=CARTESIAN_POINT('Ctrl Pts',(-0.962485392528368,-0.317195968905306,
-1.33211611256184));
#13759=CARTESIAN_POINT('Ctrl Pts',(-0.985600426557816,-0.33909093068465,
-1.31521005565926));
#13760=CARTESIAN_POINT('Ctrl Pts',(-1.03253285680459,-0.373586846396559,
-1.27866649102984));
#13761=CARTESIAN_POINT('Ctrl Pts',(-1.05871835910697,-0.388086240756494,
-1.25722555095714));
#13762=CARTESIAN_POINT('Ctrl Pts',(-1.11153475808518,-0.407068917407805,
-1.2107812086231));
#13763=CARTESIAN_POINT('Ctrl Pts',(-1.13814686046673,-0.411552957311693,
-1.18575674747573));
#13764=CARTESIAN_POINT('Ctrl Pts',(-1.18575674747573,-0.411552957311693,
-1.13814686046673));
#13765=CARTESIAN_POINT('Ctrl Pts',(-1.2107812086231,-0.407068917407805,
-1.11153475808518));
#13766=CARTESIAN_POINT('Ctrl Pts',(-1.25722555095714,-0.388086240756494,
-1.05871835910697));
#13767=CARTESIAN_POINT('Ctrl Pts',(-1.27866649102984,-0.373586846396559,
-1.03253285680459));
#13768=CARTESIAN_POINT('Ctrl Pts',(-1.31521005565926,-0.33909093068465,
-0.985600426557816));
#13769=CARTESIAN_POINT('Ctrl Pts',(-1.33211611256184,-0.317195968905306,
-0.962485392528369));
#13770=CARTESIAN_POINT('Ctrl Pts',(-1.36127834356734,-0.266264900654909,
-0.920778333482565));
#13771=CARTESIAN_POINT('Ctrl Pts',(-1.3735491215176,-0.237231147975234,
-0.902193646979983));
#13772=CARTESIAN_POINT('Ctrl Pts',(-1.39550172959303,-0.166543350814306,
-0.867957148219442));
#13773=CARTESIAN_POINT('Ctrl Pts',(-1.40380622184538,-0.123401821157026,
-0.854205272175555));
#13774=CARTESIAN_POINT('Ctrl Pts',(-1.40825612658882,-0.07938,-0.846804978391753));
#13775=CARTESIAN_POINT('Origin',(-1.18440385848747,-0.07938,-1.18440385848747));
#13776=CARTESIAN_POINT('Origin',(0.,-0.07938,0.));
#13777=CARTESIAN_POINT('',(-0.397005914195118,-0.07938,-1.59456899932179));
#13778=CARTESIAN_POINT('Origin',(0.,-0.07938,0.));
#13779=CARTESIAN_POINT('Origin',(1.11022302462516E-16,-0.07938,-1.675));
#13780=CARTESIAN_POINT('Origin',(1.11022302462516E-16,0.,-1.675));
#13781=CARTESIAN_POINT('',(0.397005914195118,-0.07938,-1.59456899932179));
#13782=CARTESIAN_POINT('Ctrl Pts',(0.397005914195119,-0.0793800000000001,
-1.59456899932179));
#13783=CARTESIAN_POINT('Ctrl Pts',(0.388626558458099,-0.123401821157026,
-1.59665523941937));
#13784=CARTESIAN_POINT('Ctrl Pts',(0.373030350867485,-0.166543350814306,
-1.60050712143809));
#13785=CARTESIAN_POINT('Ctrl Pts',(0.333298652394954,-0.237231147975234,
-1.60919314384089));
#13786=CARTESIAN_POINT('Ctrl Pts',(0.311480544243686,-0.266264900654909,
-1.61365775139403));
#13787=CARTESIAN_POINT('Ctrl Pts',(0.261368388670537,-0.317195968905306,
-1.62252828437015));
#13788=CARTESIAN_POINT('Ctrl Pts',(0.233069203882014,-0.33909093068465,
-1.62691869420078));
#13789=CARTESIAN_POINT('Ctrl Pts',(0.174042761838763,-0.373586846396559,
-1.63426473152765));
#13790=CARTESIAN_POINT('Ctrl Pts',(0.140365781471549,-0.388086240756494,
-1.63761964365402));
#13791=CARTESIAN_POINT('Ctrl Pts',(0.0701778381840612,-0.407068917407805,
-1.64212536811722));
#13792=CARTESIAN_POINT('Ctrl Pts',(0.0336652739555916,-0.411552957311693,
-1.643248));
#13793=CARTESIAN_POINT('Ctrl Pts',(-0.0336652739555915,-0.411552957311693,
-1.643248));
#13794=CARTESIAN_POINT('Ctrl Pts',(-0.0701778381840612,-0.407068917407805,
-1.64212536811722));
#13795=CARTESIAN_POINT('Ctrl Pts',(-0.140365781471549,-0.388086240756494,
-1.63761964365402));
#13796=CARTESIAN_POINT('Ctrl Pts',(-0.174042761838764,-0.373586846396559,
-1.63426473152765));
#13797=CARTESIAN_POINT('Ctrl Pts',(-0.233069203882014,-0.33909093068465,
-1.62691869420078));
#13798=CARTESIAN_POINT('Ctrl Pts',(-0.261368388670536,-0.317195968905306,
-1.62252828437015));
#13799=CARTESIAN_POINT('Ctrl Pts',(-0.311480544243686,-0.266264900654908,
-1.61365775139403));
#13800=CARTESIAN_POINT('Ctrl Pts',(-0.333298652394954,-0.237231147975234,
-1.60919314384089));
#13801=CARTESIAN_POINT('Ctrl Pts',(-0.373030350867485,-0.166543350814306,
-1.60050712143809));
#13802=CARTESIAN_POINT('Ctrl Pts',(-0.388626558458099,-0.123401821157026,
-1.59665523941937));
#13803=CARTESIAN_POINT('Ctrl Pts',(-0.397005914195118,-0.07938,-1.59456899932179));
#13804=CARTESIAN_POINT('Origin',(1.11022302462516E-16,-0.07938,-1.675));
#13805=CARTESIAN_POINT('Origin',(0.,-0.07938,0.));
#13806=CARTESIAN_POINT('',(0.846804978391753,-0.07938,-1.40825612658882));
#13807=CARTESIAN_POINT('Origin',(0.,-0.07938,0.));
#13808=CARTESIAN_POINT('Origin',(1.18440385848747,-0.07938,-1.18440385848747));
#13809=CARTESIAN_POINT('Origin',(1.18440385848747,0.,-1.18440385848747));
#13810=CARTESIAN_POINT('',(1.40825612658882,-0.07938,-0.846804978391753));
#13811=CARTESIAN_POINT('Ctrl Pts',(1.40825612658882,-0.0793800000000001,
-0.846804978391753));
#13812=CARTESIAN_POINT('Ctrl Pts',(1.40380622184538,-0.123401821157026,
-0.854205272175555));
#13813=CARTESIAN_POINT('Ctrl Pts',(1.39550172959303,-0.166543350814306,
-0.867957148219442));
#13814=CARTESIAN_POINT('Ctrl Pts',(1.3735491215176,-0.237231147975234,-0.902193646979983));
#13815=CARTESIAN_POINT('Ctrl Pts',(1.36127834356734,-0.266264900654908,
-0.920778333482565));
#13816=CARTESIAN_POINT('Ctrl Pts',(1.33211611256184,-0.317195968905306,
-0.962485392528369));
#13817=CARTESIAN_POINT('Ctrl Pts',(1.31521005565926,-0.33909093068465,-0.985600426557816));
#13818=CARTESIAN_POINT('Ctrl Pts',(1.27866649102984,-0.373586846396559,
-1.03253285680459));
#13819=CARTESIAN_POINT('Ctrl Pts',(1.25722555095714,-0.388086240756494,
-1.05871835910697));
#13820=CARTESIAN_POINT('Ctrl Pts',(1.2107812086231,-0.407068917407805,-1.11153475808518));
#13821=CARTESIAN_POINT('Ctrl Pts',(1.18575674747573,-0.411552957311693,
-1.13814686046673));
#13822=CARTESIAN_POINT('Ctrl Pts',(1.13814686046673,-0.411552957311693,
-1.18575674747573));
#13823=CARTESIAN_POINT('Ctrl Pts',(1.11153475808518,-0.407068917407805,
-1.2107812086231));
#13824=CARTESIAN_POINT('Ctrl Pts',(1.05871835910697,-0.388086240756494,
-1.25722555095714));
#13825=CARTESIAN_POINT('Ctrl Pts',(1.03253285680459,-0.373586846396559,
-1.27866649102984));
#13826=CARTESIAN_POINT('Ctrl Pts',(0.985600426557816,-0.33909093068465,
-1.31521005565926));
#13827=CARTESIAN_POINT('Ctrl Pts',(0.962485392528369,-0.317195968905306,
-1.33211611256184));
#13828=CARTESIAN_POINT('Ctrl Pts',(0.920778333482565,-0.266264900654909,
-1.36127834356734));
#13829=CARTESIAN_POINT('Ctrl Pts',(0.902193646979983,-0.237231147975234,
-1.3735491215176));
#13830=CARTESIAN_POINT('Ctrl Pts',(0.867957148219442,-0.166543350814306,
-1.39550172959303));
#13831=CARTESIAN_POINT('Ctrl Pts',(0.854205272175555,-0.123401821157026,
-1.40380622184538));
#13832=CARTESIAN_POINT('Ctrl Pts',(0.846804978391753,-0.0793800000000001,
-1.40825612658882));
#13833=CARTESIAN_POINT('Origin',(1.18440385848747,-0.07938,-1.18440385848747));
#13834=CARTESIAN_POINT('Origin',(0.,-0.27783,0.));
#13835=CARTESIAN_POINT('',(-1.643248,-0.47628,2.01239840340529E-16));
#13836=CARTESIAN_POINT('Origin',(0.,-0.47628,0.));
#13837=CARTESIAN_POINT('',(-1.643248,-0.27783,2.01239840340529E-16));
#13838=CARTESIAN_POINT('',(1.59456899932179,-0.07938,0.397005914195118));
#13839=CARTESIAN_POINT('Origin',(0.,-0.07938,0.));
#13840=CARTESIAN_POINT('',(1.59456899932179,-0.07938,-0.397005914195118));
#13841=CARTESIAN_POINT('Ctrl Pts',(1.59456899932179,-0.0793800000000001,
0.397005914195118));
#13842=CARTESIAN_POINT('Ctrl Pts',(1.59665523941937,-0.123401821157026,
0.388626558458099));
#13843=CARTESIAN_POINT('Ctrl Pts',(1.60050712143809,-0.166543350814306,
0.373030350867485));
#13844=CARTESIAN_POINT('Ctrl Pts',(1.60919314384089,-0.237231147975234,
0.333298652394954));
#13845=CARTESIAN_POINT('Ctrl Pts',(1.61365775139403,-0.266264900654909,
0.311480544243686));
#13846=CARTESIAN_POINT('Ctrl Pts',(1.62252828437015,-0.317195968905306,
0.261368388670537));
#13847=CARTESIAN_POINT('Ctrl Pts',(1.62691869420078,-0.33909093068465,0.233069203882014));
#13848=CARTESIAN_POINT('Ctrl Pts',(1.63426473152765,-0.373586846396559,
0.174042761838764));
#13849=CARTESIAN_POINT('Ctrl Pts',(1.63761964365402,-0.388086240756494,
0.140365781471549));
#13850=CARTESIAN_POINT('Ctrl Pts',(1.64212536811722,-0.407068917407805,
0.0701778381840612));
#13851=CARTESIAN_POINT('Ctrl Pts',(1.643248,-0.411552957311693,0.0336652739555916));
#13852=CARTESIAN_POINT('Ctrl Pts',(1.643248,-0.411552957311693,-0.0336652739555916));
#13853=CARTESIAN_POINT('Ctrl Pts',(1.64212536811722,-0.407068917407805,
-0.0701778381840612));
#13854=CARTESIAN_POINT('Ctrl Pts',(1.63761964365402,-0.388086240756494,
-0.140365781471549));
#13855=CARTESIAN_POINT('Ctrl Pts',(1.63426473152765,-0.373586846396559,
-0.174042761838764));
#13856=CARTESIAN_POINT('Ctrl Pts',(1.62691869420078,-0.33909093068465,-0.233069203882014));
#13857=CARTESIAN_POINT('Ctrl Pts',(1.62252828437015,-0.317195968905306,
-0.261368388670537));
#13858=CARTESIAN_POINT('Ctrl Pts',(1.61365775139403,-0.266264900654909,
-0.311480544243686));
#13859=CARTESIAN_POINT('Ctrl Pts',(1.60919314384089,-0.237231147975234,
-0.333298652394954));
#13860=CARTESIAN_POINT('Ctrl Pts',(1.60050712143809,-0.166543350814306,
-0.373030350867485));
#13861=CARTESIAN_POINT('Ctrl Pts',(1.59665523941937,-0.123401821157026,
-0.388626558458099));
#13862=CARTESIAN_POINT('Ctrl Pts',(1.59456899932179,-0.07938,-0.397005914195118));
#13863=CARTESIAN_POINT('Origin',(0.,-0.07938,0.));
#13864=CARTESIAN_POINT('Origin',(0.,-0.07938,0.));
#13865=CARTESIAN_POINT('Origin',(1.675,-0.07938,0.));
#13866=CARTESIAN_POINT('Origin',(1.675,0.,0.));
#13867=CARTESIAN_POINT('Origin',(1.675,-0.07938,0.));
#13868=CARTESIAN_POINT('Origin',(0.,-0.47628,0.));
#13869=CARTESIAN_POINT('Origin',(0.,-0.07938,0.));
#13870=CARTESIAN_POINT('',(0.,0.,0.));
#13871=CARTESIAN_POINT('Origin',(1.70469,0.695,0.));
#13872=CARTESIAN_POINT('',(-1.70469,0.695,-2.0876431520385E-16));
#13873=CARTESIAN_POINT('Origin',(0.,0.695,0.));
#13874=CARTESIAN_POINT('',(-1.65031,0.695,-2.02104685910087E-16));
#13875=CARTESIAN_POINT('Origin',(0.,0.695,0.));
#13876=CARTESIAN_POINT('Origin',(0.,0.6575,0.));
#13877=CARTESIAN_POINT('',(-1.70469,0.62,-2.0876431520385E-16));
#13878=CARTESIAN_POINT('Origin',(0.,0.62,0.));
#13879=CARTESIAN_POINT('',(-1.70469,0.6575,-2.0876431520385E-16));
#13880=CARTESIAN_POINT('Origin',(1.65031,0.62,0.));
#13881=CARTESIAN_POINT('',(-1.65031,0.62,-2.02104685910087E-16));
#13882=CARTESIAN_POINT('Origin',(0.,0.62,0.));
#13883=CARTESIAN_POINT('Origin',(0.,0.6575,0.));
#13884=CARTESIAN_POINT('',(-1.65031,0.6575,-2.02104685910087E-16));
#13885=CARTESIAN_POINT('Origin',(1.70469,-0.62,0.));
#13886=CARTESIAN_POINT('',(-1.70469,-0.62,-2.0876431520385E-16));
#13887=CARTESIAN_POINT('Origin',(0.,-0.62,0.));
#13888=CARTESIAN_POINT('',(-1.65031,-0.62,-2.02104685910087E-16));
#13889=CARTESIAN_POINT('Origin',(0.,-0.62,0.));
#13890=CARTESIAN_POINT('Origin',(0.,-0.6575,0.));
#13891=CARTESIAN_POINT('',(-1.70469,-0.695,-2.0876431520385E-16));
#13892=CARTESIAN_POINT('Origin',(0.,-0.695,0.));
#13893=CARTESIAN_POINT('',(-1.70469,-0.6575,-2.0876431520385E-16));
#13894=CARTESIAN_POINT('Origin',(1.65031,-0.695,0.));
#13895=CARTESIAN_POINT('',(-1.65031,-0.695,-2.02104685910087E-16));
#13896=CARTESIAN_POINT('Origin',(0.,-0.695,0.));
#13897=CARTESIAN_POINT('Origin',(0.,-0.6575,0.));
#13898=CARTESIAN_POINT('',(-1.65031,-0.6575,-2.02104685910087E-16));
#13899=CARTESIAN_POINT('',(0.,0.,0.));
#13900=CARTESIAN_POINT('',(0.,0.,0.));
#13901=CARTESIAN_POINT('',(0.,0.,0.));
#13902=CARTESIAN_POINT('',(0.,0.,0.));
#13903=CARTESIAN_POINT('',(0.,0.,0.));
#13904=CARTESIAN_POINT('',(0.,0.,0.));
#13905=CARTESIAN_POINT('Origin',(0.375,0.5,0.));
#13906=CARTESIAN_POINT('',(-0.375,0.5,-4.59242549680257E-17));
#13907=CARTESIAN_POINT('Origin',(0.,0.5,0.));
#13908=CARTESIAN_POINT('Origin',(0.,0.475,0.));
#13909=CARTESIAN_POINT('',(-0.425,0.45,-5.20474889637625E-17));
#13910=CARTESIAN_POINT('Origin',(0.,0.45,0.));
#13911=CARTESIAN_POINT('',(-0.4,0.475,-4.89858719658941E-17));
#13912=CARTESIAN_POINT('Origin',(0.,0.24,0.));
#13913=CARTESIAN_POINT('',(-0.425,0.0299999999999998,-5.20474889637625E-17));
#13914=CARTESIAN_POINT('Origin',(0.,0.0299999999999998,0.));
#13915=CARTESIAN_POINT('',(-0.425,0.24,-5.20474889637625E-17));
#13916=CARTESIAN_POINT('Origin',(0.,0.0150000000000001,0.));
#13917=CARTESIAN_POINT('',(-0.395,4.85722573273506E-17,-4.83735485663204E-17));
#13918=CARTESIAN_POINT('Origin',(0.,0.,0.));
#13919=CARTESIAN_POINT('',(-0.41,0.0150000000000001,-5.02105187650415E-17));
#13920=CARTESIAN_POINT('Origin',(0.27,0.,0.));
#13921=CARTESIAN_POINT('',(-0.27,0.,-3.30654635769785E-17));
#13922=CARTESIAN_POINT('Origin',(0.,0.,0.));
#13923=CARTESIAN_POINT('Origin',(0.,-0.02,0.));
#13924=CARTESIAN_POINT('',(-0.24505,-0.0498999999999999,3.00099698131059E-17));
#13925=CARTESIAN_POINT('Origin',(0.,-0.0498999999999999,0.));
#13926=CARTESIAN_POINT('',(-0.26,-0.02,-3.18408167778312E-17));
#13927=CARTESIAN_POINT('Origin',(0.,-0.995,0.));
#13928=CARTESIAN_POINT('',(-0.24505,-1.95495,3.00099698131059E-17));
#13929=CARTESIAN_POINT('Origin',(0.,-1.95495,0.));
#13930=CARTESIAN_POINT('',(-0.24505,-0.995,-3.00099698131059E-17));
#13931=CARTESIAN_POINT('Origin',(0.,-1.975,0.));
#13932=CARTESIAN_POINT('',(-0.2,-2.,-2.44929359829471E-17));
#13933=CARTESIAN_POINT('Origin',(0.,-2.,0.));
#13934=CARTESIAN_POINT('',(-0.225,-1.975,-2.75545529808154E-17));
#13935=CARTESIAN_POINT('Origin',(0.,-2.,0.));
#13936=CARTESIAN_POINT('Origin',(0.115470053837925,-0.5,-0.2));
#13937=CARTESIAN_POINT('',(0.23094010767585,-0.5,0.));
#13938=CARTESIAN_POINT('',(0.115470053837925,-0.5,-0.2));
#13939=CARTESIAN_POINT('',(0.23094010767585,-0.5,0.));
#13940=CARTESIAN_POINT('',(0.115470053837925,-0.8,-0.2));
#13941=CARTESIAN_POINT('',(0.115470053837925,-0.5,-0.2));
#13942=CARTESIAN_POINT('',(0.23094010767585,-0.8,0.));
#13943=CARTESIAN_POINT('',(0.23094010767585,-0.8,0.));
#13944=CARTESIAN_POINT('',(0.23094010767585,-0.5,0.));
#13945=CARTESIAN_POINT('Origin',(-0.115470053837925,-0.5,-0.2));
#13946=CARTESIAN_POINT('',(-0.115470053837925,-0.5,-0.2));
#13947=CARTESIAN_POINT('',(0.115470053837925,-0.5,-0.2));
#13948=CARTESIAN_POINT('',(-0.115470053837925,-0.8,-0.2));
#13949=CARTESIAN_POINT('',(-0.115470053837925,-0.5,-0.2));
#13950=CARTESIAN_POINT('',(0.115470053837925,-0.8,-0.2));
#13951=CARTESIAN_POINT('Origin',(-0.23094010767585,-0.5,-2.77555756156289E-17));
#13952=CARTESIAN_POINT('',(-0.23094010767585,-0.5,-2.82820063659975E-17));
#13953=CARTESIAN_POINT('',(-0.115470053837925,-0.5,-0.2));
#13954=CARTESIAN_POINT('',(-0.23094010767585,-0.8,-2.77555756156289E-17));
#13955=CARTESIAN_POINT('',(-0.23094010767585,-0.5,-2.82820063659975E-17));
#13956=CARTESIAN_POINT('',(-0.115470053837925,-0.8,-0.2));
#13957=CARTESIAN_POINT('Origin',(-0.115470053837925,-0.5,0.2));
#13958=CARTESIAN_POINT('',(-0.115470053837925,-0.5,0.2));
#13959=CARTESIAN_POINT('',(-0.23094010767585,-0.5,-2.82820063659975E-17));
#13960=CARTESIAN_POINT('',(-0.115470053837925,-0.8,0.2));
#13961=CARTESIAN_POINT('',(-0.115470053837925,-0.5,0.2));
#13962=CARTESIAN_POINT('',(-0.23094010767585,-0.8,-2.82820063659975E-17));
#13963=CARTESIAN_POINT('Origin',(0.115470053837925,-0.5,0.2));
#13964=CARTESIAN_POINT('',(0.115470053837925,-0.5,0.2));
#13965=CARTESIAN_POINT('',(-0.115470053837925,-0.5,0.2));
#13966=CARTESIAN_POINT('',(0.115470053837925,-0.8,0.2));
#13967=CARTESIAN_POINT('',(0.115470053837925,-0.5,0.2));
#13968=CARTESIAN_POINT('',(-0.115470053837925,-0.8,0.2));
#13969=CARTESIAN_POINT('Origin',(0.23094010767585,-0.5,0.));
#13970=CARTESIAN_POINT('',(0.115470053837925,-0.5,0.2));
#13971=CARTESIAN_POINT('',(0.115470053837925,-0.8,0.2));
#13972=CARTESIAN_POINT('Origin',(0.,-0.5,0.));
#13973=CARTESIAN_POINT('Origin',(0.,-0.8,0.));
#13974=CARTESIAN_POINT('',(0.,0.,0.));
#13975=CARTESIAN_POINT('Origin',(0.0866025403784439,-0.4,-0.15));
#13976=CARTESIAN_POINT('',(0.173205080756888,-0.4,0.));
#13977=CARTESIAN_POINT('',(0.0866025403784439,-0.4,-0.15));
#13978=CARTESIAN_POINT('',(0.173205080756888,-0.4,0.));
#13979=CARTESIAN_POINT('',(0.0866025403784439,-0.64,-0.15));
#13980=CARTESIAN_POINT('',(0.0866025403784439,-0.4,-0.15));
#13981=CARTESIAN_POINT('',(0.173205080756888,-0.64,0.));
#13982=CARTESIAN_POINT('',(0.173205080756888,-0.64,0.));
#13983=CARTESIAN_POINT('',(0.173205080756888,-0.4,0.));
#13984=CARTESIAN_POINT('Origin',(-0.0866025403784438,-0.4,-0.15));
#13985=CARTESIAN_POINT('',(-0.0866025403784438,-0.4,-0.15));
#13986=CARTESIAN_POINT('',(0.0866025403784439,-0.4,-0.15));
#13987=CARTESIAN_POINT('',(-0.0866025403784438,-0.64,-0.15));
#13988=CARTESIAN_POINT('',(-0.0866025403784438,-0.4,-0.15));
#13989=CARTESIAN_POINT('',(0.0866025403784439,-0.64,-0.15));
#13990=CARTESIAN_POINT('Origin',(-0.173205080756888,-0.4,-2.77555756156289E-17));
#13991=CARTESIAN_POINT('',(-0.173205080756888,-0.4,-2.12115047744981E-17));
#13992=CARTESIAN_POINT('',(-0.0866025403784438,-0.4,-0.15));
#13993=CARTESIAN_POINT('',(-0.173205080756888,-0.64,-2.77555756156289E-17));
#13994=CARTESIAN_POINT('',(-0.173205080756888,-0.4,-2.12115047744981E-17));
#13995=CARTESIAN_POINT('',(-0.0866025403784438,-0.64,-0.15));
#13996=CARTESIAN_POINT('Origin',(-0.0866025403784439,-0.4,0.15));
#13997=CARTESIAN_POINT('',(-0.0866025403784439,-0.4,0.15));
#13998=CARTESIAN_POINT('',(-0.173205080756888,-0.4,-2.12115047744981E-17));
#13999=CARTESIAN_POINT('',(-0.0866025403784439,-0.64,0.15));
#14000=CARTESIAN_POINT('',(-0.0866025403784439,-0.4,0.15));
#14001=CARTESIAN_POINT('',(-0.173205080756888,-0.64,-2.12115047744981E-17));
#14002=CARTESIAN_POINT('Origin',(0.0866025403784439,-0.4,0.15));
#14003=CARTESIAN_POINT('',(0.0866025403784439,-0.4,0.15));
#14004=CARTESIAN_POINT('',(-0.0866025403784439,-0.4,0.15));
#14005=CARTESIAN_POINT('',(0.0866025403784439,-0.64,0.15));
#14006=CARTESIAN_POINT('',(0.0866025403784439,-0.4,0.15));
#14007=CARTESIAN_POINT('',(-0.0866025403784439,-0.64,0.15));
#14008=CARTESIAN_POINT('Origin',(0.173205080756888,-0.4,0.));
#14009=CARTESIAN_POINT('',(0.0866025403784439,-0.4,0.15));
#14010=CARTESIAN_POINT('',(0.0866025403784439,-0.64,0.15));
#14011=CARTESIAN_POINT('Origin',(0.,-0.4,-2.77555756156289E-17));
#14012=CARTESIAN_POINT('Origin',(0.,-0.64,-2.77555756156289E-17));
#14013=CARTESIAN_POINT('Origin',(0.,-1.,0.));
#14014=CARTESIAN_POINT('',(-0.1954,-1.,2.39295984553393E-17));
#14015=CARTESIAN_POINT('Origin',(0.,-1.,0.));
#14016=CARTESIAN_POINT('Origin',(0.3,0.4,0.));
#14017=CARTESIAN_POINT('',(-0.3,0.4,-3.67394039744206E-17));
#14018=CARTESIAN_POINT('Origin',(0.,0.4,0.));
#14019=CARTESIAN_POINT('Origin',(0.,0.375,0.));
#14020=CARTESIAN_POINT('',(-0.35,0.35,-4.28626379701573E-17));
#14021=CARTESIAN_POINT('Origin',(0.,0.35,0.));
#14022=CARTESIAN_POINT('',(-0.325,0.375,-3.9801020972289E-17));
#14023=CARTESIAN_POINT('Origin',(0.,0.19,0.));
#14024=CARTESIAN_POINT('',(-0.35,0.03,-4.28626379701574E-17));
#14025=CARTESIAN_POINT('Origin',(0.,0.03,0.));
#14026=CARTESIAN_POINT('',(-0.35,0.19,-4.28626379701574E-17));
#14027=CARTESIAN_POINT('Origin',(0.,0.0149999999999999,0.));
#14028=CARTESIAN_POINT('',(-0.32,-3.29597460435593E-17,-3.91886975727153E-17));
#14029=CARTESIAN_POINT('Origin',(0.,0.,0.));
#14030=CARTESIAN_POINT('',(-0.335,0.0149999999999999,-4.10256677714363E-17));
#14031=CARTESIAN_POINT('Origin',(0.22,0.,0.));
#14032=CARTESIAN_POINT('',(-0.22,-6.93889390390723E-18,-2.69422295812418E-17));
#14033=CARTESIAN_POINT('Origin',(0.,0.,0.));
#14034=CARTESIAN_POINT('Origin',(0.,-0.02,0.));
#14035=CARTESIAN_POINT('',(-0.1954,-0.0492,2.39295984553393E-17));
#14036=CARTESIAN_POINT('Origin',(0.,-0.0492,0.));
#14037=CARTESIAN_POINT('',(-0.21,-0.02,-2.57175827820944E-17));
#14038=CARTESIAN_POINT('Origin',(0.,-0.8,0.));
#14039=CARTESIAN_POINT('',(-0.1954,-0.8,-2.39295984553393E-17));
#14040=CARTESIAN_POINT('',(0.,0.,0.));
#14041=CARTESIAN_POINT('',(0.,0.,0.));
#14042=CARTESIAN_POINT('',(0.,0.,0.));
#14043=CARTESIAN_POINT('',(0.,0.,0.));
#14044=CARTESIAN_POINT('',(0.,0.,0.));
#14045=CARTESIAN_POINT('',(0.,0.,0.));
#14046=CARTESIAN_POINT('',(0.,0.,0.));
#14047=CARTESIAN_POINT('',(0.,0.,0.));
#14048=CARTESIAN_POINT('',(0.,0.,0.));
#14049=CARTESIAN_POINT('',(0.,0.,0.));
#14050=CARTESIAN_POINT('',(0.,0.,0.));
#14051=CARTESIAN_POINT('',(0.,0.,0.));
#14052=CARTESIAN_POINT('',(0.,0.,0.));
#14053=CARTESIAN_POINT('',(0.,0.,0.));
#14054=CARTESIAN_POINT('',(0.,0.,0.));
#14055=CARTESIAN_POINT('',(-2.7,-7.,1.8));
#14056=CARTESIAN_POINT('',(2.7,-7.,1.8));
#14057=CARTESIAN_POINT('',(0.,-7.,7.));
#14058=CARTESIAN_POINT('',(2.,-8.1,7.));
#14059=CARTESIAN_POINT('',(2.22044604925031E-16,-8.1,9.));
#14060=CARTESIAN_POINT('',(-2.,-8.1,7.));
#14061=CARTESIAN_POINT('',(-4.44089209850063E-16,-8.1,5.));
#14062=CARTESIAN_POINT('',(2.,-5.9,7.));
#14063=CARTESIAN_POINT('',(2.22044604925031E-16,-5.9,9.));
#14064=CARTESIAN_POINT('',(-2.,-5.9,7.));
#14065=CARTESIAN_POINT('',(0.,-5.9,5.));
#14066=CARTESIAN_POINT('',(-2.7,7.,1.8));
#14067=CARTESIAN_POINT('',(2.7,7.,1.8));
#14068=CARTESIAN_POINT('',(0.,7.,7.));
#14069=CARTESIAN_POINT('',(2.,5.9,7.));
#14070=CARTESIAN_POINT('',(4.44089209850063E-16,5.9,9.));
#14071=CARTESIAN_POINT('',(-2.,5.9,7.));
#14072=CARTESIAN_POINT('',(0.,5.9,5.));
#14073=CARTESIAN_POINT('',(2.,8.1,7.));
#14074=CARTESIAN_POINT('',(2.22044604925031E-16,8.1,9.));
#14075=CARTESIAN_POINT('',(-2.,8.1,7.));
#14076=CARTESIAN_POINT('',(-4.44089209850063E-16,8.1,5.));
#14077=CARTESIAN_POINT('',(0.,0.,7.));
#14078=CARTESIAN_POINT('',(1.83847763108502,-1.1,8.83847763108502));
#14079=CARTESIAN_POINT('',(-1.83847763108502,-1.1,8.83847763108502));
#14080=CARTESIAN_POINT('',(-1.83847763108502,-1.1,5.16152236891498));
#14081=CARTESIAN_POINT('',(1.83847763108502,-1.1,5.16152236891498));
#14082=CARTESIAN_POINT('',(1.83847763108502,1.1,8.83847763108502));
#14083=CARTESIAN_POINT('',(-1.83847763108502,1.1,8.83847763108502));
#14084=CARTESIAN_POINT('',(-1.83847763108502,1.1,5.16152236891498));
#14085=CARTESIAN_POINT('',(1.83847763108502,1.1,5.16152236891498));
#14086=CARTESIAN_POINT('',(8.6,-1.4,2.2));
#14087=CARTESIAN_POINT('',(8.6,1.4,2.2));
#14088=CARTESIAN_POINT('',(11.4,-1.4,2.2));
#14089=CARTESIAN_POINT('',(11.4,1.4,2.2));
#14090=CARTESIAN_POINT('',(10.,-1.7,4.9));
#14091=CARTESIAN_POINT('',(10.,1.7,4.9));
#14092=CARTESIAN_POINT('',(-4.4,-3.4,1.5));
#14093=CARTESIAN_POINT('',(-4.4,3.4,1.5));
#14094=CARTESIAN_POINT('',(4.4,-3.4,1.5));
#14095=CARTESIAN_POINT('',(4.4,3.4,1.5));
#14096=CARTESIAN_POINT('',(0.,0.,0.));
#14097=CARTESIAN_POINT('',(0.,0.,0.));
#14098=CARTESIAN_POINT('Origin',(0.,2.5,7.));
#14099=CARTESIAN_POINT('',(-0.6,9.,7.));
#14100=CARTESIAN_POINT('Origin',(0.,9.,7.));
#14101=CARTESIAN_POINT('',(-0.6,2.5,7.));
#14102=CARTESIAN_POINT('',(-0.6,2.5,7.));
#14103=CARTESIAN_POINT('Origin',(0.,2.5,7.));
#14104=CARTESIAN_POINT('Origin',(0.,9.,7.));
#14105=CARTESIAN_POINT('Origin',(0.,-11.,7.));
#14106=CARTESIAN_POINT('',(-0.6,-2.5,7.));
#14107=CARTESIAN_POINT('Origin',(0.,-2.5,7.));
#14108=CARTESIAN_POINT('',(-0.6,-11.,7.));
#14109=CARTESIAN_POINT('',(-0.6,-11.,7.));
#14110=CARTESIAN_POINT('Origin',(0.,-11.,7.));
#14111=CARTESIAN_POINT('Origin',(0.,-11.,7.));
#14112=CARTESIAN_POINT('Origin',(0.,-2.5,7.));
#14113=CARTESIAN_POINT('',(-1.,2.5,7.));
#14114=CARTESIAN_POINT('Origin',(0.,2.5,7.));
#14115=CARTESIAN_POINT('',(-1.,-2.5,7.));
#14116=CARTESIAN_POINT('',(-1.,-2.5,7.));
#14117=CARTESIAN_POINT('Origin',(0.,-2.5,7.));
#14118=CARTESIAN_POINT('Origin',(0.,2.5,7.));
#14119=CARTESIAN_POINT('Origin',(0.,-2.5,7.));
#14120=CARTESIAN_POINT('',(0.,0.,0.));
#14121=CARTESIAN_POINT('Origin',(0.,-6.5,7.));
#14122=CARTESIAN_POINT('',(-0.605,-2.5,7.));
#14123=CARTESIAN_POINT('Origin',(0.,-2.5,7.));
#14124=CARTESIAN_POINT('',(-0.605,-6.5,7.));
#14125=CARTESIAN_POINT('',(-0.605,-6.5,7.));
#14126=CARTESIAN_POINT('Origin',(0.,-6.5,7.));
#14127=CARTESIAN_POINT('Origin',(0.,-6.5,7.));
#14128=CARTESIAN_POINT('',(-0.9,-2.5,7.));
#14129=CARTESIAN_POINT('Origin',(0.,-2.5,7.));
#14130=CARTESIAN_POINT('',(-0.9,-6.5,7.));
#14131=CARTESIAN_POINT('',(-0.9,-6.5,7.));
#14132=CARTESIAN_POINT('Origin',(0.,-6.5,7.));
#14133=CARTESIAN_POINT('Origin',(0.,-2.5,7.));
#14134=CARTESIAN_POINT('Origin',(0.,-6.5,7.));
#14135=CARTESIAN_POINT('',(0.,0.,0.));
#14136=CARTESIAN_POINT('Origin',(0.,2.5,7.));
#14137=CARTESIAN_POINT('',(-0.605,6.5,7.));
#14138=CARTESIAN_POINT('Origin',(0.,6.5,7.));
#14139=CARTESIAN_POINT('',(-0.605,2.5,7.));
#14140=CARTESIAN_POINT('',(-0.605,2.5,7.));
#14141=CARTESIAN_POINT('Origin',(0.,2.5,7.));
#14142=CARTESIAN_POINT('Origin',(0.,2.5,7.));
#14143=CARTESIAN_POINT('',(-0.9,6.5,7.));
#14144=CARTESIAN_POINT('Origin',(0.,6.5,7.));
#14145=CARTESIAN_POINT('',(-0.9,2.5,7.));
#14146=CARTESIAN_POINT('',(-0.9,2.5,7.));
#14147=CARTESIAN_POINT('Origin',(0.,2.5,7.));
#14148=CARTESIAN_POINT('Origin',(0.,6.5,7.));
#14149=CARTESIAN_POINT('Origin',(0.,2.5,7.));
#14150=CARTESIAN_POINT('',(0.,0.,0.));
#14151=CARTESIAN_POINT('Origin',(0.,-8.6,7.59));
#14152=CARTESIAN_POINT('',(0.133884278389956,-8.76178689687364,7.59));
#14153=CARTESIAN_POINT('',(0.133884278389956,-8.43821310312636,7.59));
#14154=CARTESIAN_POINT('',(0.133884278389956,-9.,7.59));
#14155=CARTESIAN_POINT('Origin',(0.,-8.6,7.59));
#14156=CARTESIAN_POINT('Origin',(0.,-8.6,7.59));
#14157=CARTESIAN_POINT('',(-0.133884278389956,-8.76178689687364,7.59));
#14158=CARTESIAN_POINT('Ctrl Pts',(-0.133884278389955,-8.76178689687364,
7.59));
#14159=CARTESIAN_POINT('Ctrl Pts',(-0.118254395260799,-8.77472116821763,
7.59354677224418));
#14160=CARTESIAN_POINT('Ctrl Pts',(-0.100109787682298,-8.78579931658744,
7.59698224789957));
#14161=CARTESIAN_POINT('Ctrl Pts',(-0.054829872132519,-8.80463856105443,
7.6030741628997));
#14162=CARTESIAN_POINT('Ctrl Pts',(-0.0266020595922903,-8.81,7.605));
#14163=CARTESIAN_POINT('Ctrl Pts',(0.0266020595922903,-8.81,7.605));
#14164=CARTESIAN_POINT('Ctrl Pts',(0.0548298721325189,-8.80463856105443,
7.6030741628997));
#14165=CARTESIAN_POINT('Ctrl Pts',(0.100109787682298,-8.78579931658744,
7.59698224789957));
#14166=CARTESIAN_POINT('Ctrl Pts',(0.118254395260801,-8.77472116821763,
7.59354677224418));
#14167=CARTESIAN_POINT('Ctrl Pts',(0.133884278389955,-8.76178689687364,
7.59));
#14168=CARTESIAN_POINT('',(-0.21,-8.6,7.59));
#14169=CARTESIAN_POINT('Origin',(0.,-8.6,7.59));
#14170=CARTESIAN_POINT('',(-0.21,-8.6,7.97770138590472));
#14171=CARTESIAN_POINT('',(-0.21,-8.6,7.59));
#14172=CARTESIAN_POINT('',(0.21,-8.6,7.97770138590472));
#14173=CARTESIAN_POINT('Ctrl Pts',(0.21,-8.6,7.97770138590472));
#14174=CARTESIAN_POINT('Ctrl Pts',(0.21,-8.62645388258982,7.97770138590472));
#14175=CARTESIAN_POINT('Ctrl Pts',(0.204697017125528,-8.65461525830868,
7.97888646613217));
#14176=CARTESIAN_POINT('Ctrl Pts',(0.183241751515529,-8.70633042130174,
7.98312869991148));
#14177=CARTESIAN_POINT('Ctrl Pts',(0.167093586802906,-8.72989126129544,
7.98612044796649));
#14178=CARTESIAN_POINT('Ctrl Pts',(0.129892533236543,-8.76709231486181,
7.99170645156379));
#14179=CARTESIAN_POINT('Ctrl Pts',(0.106331154992714,-8.78324147510569,
7.99466914446598));
#14180=CARTESIAN_POINT('Ctrl Pts',(0.0546141143983522,-8.80469746372443,
7.99884449237241));
#14181=CARTESIAN_POINT('Ctrl Pts',(0.0264520736824499,-8.81,8.));
#14182=CARTESIAN_POINT('Ctrl Pts',(-0.0264520736824498,-8.81,8.));
#14183=CARTESIAN_POINT('Ctrl Pts',(-0.0546141143983521,-8.80469746372443,
7.99884449237241));
#14184=CARTESIAN_POINT('Ctrl Pts',(-0.106331154992714,-8.78324147510569,
7.99466914446598));
#14185=CARTESIAN_POINT('Ctrl Pts',(-0.129892533236543,-8.76709231486181,
7.99170645156379));
#14186=CARTESIAN_POINT('Ctrl Pts',(-0.167093586802906,-8.72989126129544,
7.98612044796649));
#14187=CARTESIAN_POINT('Ctrl Pts',(-0.183241751515529,-8.70633042130174,
7.98312869991148));
#14188=CARTESIAN_POINT('Ctrl Pts',(-0.204697017125528,-8.65461525830868,
7.97888646613217));
#14189=CARTESIAN_POINT('Ctrl Pts',(-0.21,-8.62645388258982,7.97770138590472));
#14190=CARTESIAN_POINT('Ctrl Pts',(-0.21,-8.6,7.97770138590472));
#14191=CARTESIAN_POINT('Ctrl Pts',(-0.21,-8.6,7.97770138590472));
#14192=CARTESIAN_POINT('Ctrl Pts',(-0.21,-8.57354611741017,7.97770138590472));
#14193=CARTESIAN_POINT('Ctrl Pts',(-0.204697017125528,-8.54538474169131,
7.97888646613217));
#14194=CARTESIAN_POINT('Ctrl Pts',(-0.183241751515529,-8.49366957869826,
7.98312869991148));
#14195=CARTESIAN_POINT('Ctrl Pts',(-0.167093586802906,-8.47010873870456,
7.98612044796649));
#14196=CARTESIAN_POINT('Ctrl Pts',(-0.129892533236543,-8.43290768513819,
7.99170645156379));
#14197=CARTESIAN_POINT('Ctrl Pts',(-0.106331154992714,-8.41675852489431,
7.99466914446598));
#14198=CARTESIAN_POINT('Ctrl Pts',(-0.0546141143983522,-8.39530253627557,
7.99884449237241));
#14199=CARTESIAN_POINT('Ctrl Pts',(-0.0264520736824499,-8.39,8.));
#14200=CARTESIAN_POINT('Ctrl Pts',(0.0264520736824499,-8.39,8.));
#14201=CARTESIAN_POINT('Ctrl Pts',(0.0546141143983517,-8.39530253627557,
7.99884449237241));
#14202=CARTESIAN_POINT('Ctrl Pts',(0.106331154992713,-8.41675852489431,
7.99466914446598));
#14203=CARTESIAN_POINT('Ctrl Pts',(0.129892533236543,-8.43290768513819,
7.99170645156379));
#14204=CARTESIAN_POINT('Ctrl Pts',(0.167093586802906,-8.47010873870456,
7.98612044796649));
#14205=CARTESIAN_POINT('Ctrl Pts',(0.183241751515529,-8.49366957869826,
7.98312869991148));
#14206=CARTESIAN_POINT('Ctrl Pts',(0.204697017125528,-8.54538474169131,
7.97888646613217));
#14207=CARTESIAN_POINT('Ctrl Pts',(0.21,-8.57354611741017,7.97770138590472));
#14208=CARTESIAN_POINT('Ctrl Pts',(0.21,-8.6,7.97770138590472));
#14209=CARTESIAN_POINT('',(-0.133884278389956,-8.43821310312636,7.59));
#14210=CARTESIAN_POINT('Origin',(0.,-8.6,7.59));
#14211=CARTESIAN_POINT('Ctrl Pts',(0.133884278389955,-8.43821310312636,
7.59));
#14212=CARTESIAN_POINT('Ctrl Pts',(0.118254395260801,-8.42527883178237,
7.59354677224418));
#14213=CARTESIAN_POINT('Ctrl Pts',(0.100109787682299,-8.41420068341256,
7.59698224789957));
#14214=CARTESIAN_POINT('Ctrl Pts',(0.054829872132519,-8.39536143894557,
7.6030741628997));
#14215=CARTESIAN_POINT('Ctrl Pts',(0.0266020595922903,-8.39,7.605));
#14216=CARTESIAN_POINT('Ctrl Pts',(-0.0266020595922903,-8.39,7.605));
#14217=CARTESIAN_POINT('Ctrl Pts',(-0.0548298721325189,-8.39536143894557,
7.6030741628997));
#14218=CARTESIAN_POINT('Ctrl Pts',(-0.100109787682299,-8.41420068341256,
7.59698224789957));
#14219=CARTESIAN_POINT('Ctrl Pts',(-0.118254395260801,-8.42527883178237,
7.59354677224418));
#14220=CARTESIAN_POINT('Ctrl Pts',(-0.133884278389955,-8.43821310312636,
7.59));
#14221=CARTESIAN_POINT('Origin',(0.,-8.6,7.59));
#14222=CARTESIAN_POINT('',(-0.133884278389956,-9.,7.59));
#14223=CARTESIAN_POINT('Origin',(0.,-9.,7.));
#14224=CARTESIAN_POINT('',(-0.605,-8.2,7.));
#14225=CARTESIAN_POINT('Origin',(0.,-8.2,7.));
#14226=CARTESIAN_POINT('',(-0.605,-9.,7.));
#14227=CARTESIAN_POINT('',(-0.605,-9.,7.));
#14228=CARTESIAN_POINT('Origin',(0.,-9.,7.));
#14229=CARTESIAN_POINT('Origin',(0.,-9.,7.));
#14230=CARTESIAN_POINT('',(-1.,-8.2,7.));
#14231=CARTESIAN_POINT('Origin',(0.,-8.2,7.));
#14232=CARTESIAN_POINT('',(-1.,-9.,7.));
#14233=CARTESIAN_POINT('',(-1.,-9.,7.));
#14234=CARTESIAN_POINT('Origin',(0.,-9.,7.));
#14235=CARTESIAN_POINT('Origin',(0.,-8.2,7.));
#14236=CARTESIAN_POINT('Origin',(0.,-9.,7.));
#14237=CARTESIAN_POINT('',(0.,0.,0.));
#14238=CARTESIAN_POINT('Origin',(0.,8.6,7.59));
#14239=CARTESIAN_POINT('',(0.133884278389956,8.43821310312636,7.59));
#14240=CARTESIAN_POINT('',(0.133884278389956,8.76178689687364,7.59));
#14241=CARTESIAN_POINT('',(0.133884278389956,8.2,7.59));
#14242=CARTESIAN_POINT('Origin',(0.,8.6,7.59));
#14243=CARTESIAN_POINT('Origin',(0.,8.6,7.59));
#14244=CARTESIAN_POINT('',(-0.133884278389956,8.43821310312636,7.59));
#14245=CARTESIAN_POINT('Ctrl Pts',(-0.133884278389955,8.43821310312636,
7.59));
#14246=CARTESIAN_POINT('Ctrl Pts',(-0.1182543952608,8.42527883178237,7.59354677224418));
#14247=CARTESIAN_POINT('Ctrl Pts',(-0.100109787682298,8.41420068341256,
7.59698224789957));
#14248=CARTESIAN_POINT('Ctrl Pts',(-0.054829872132519,8.39536143894557,
7.6030741628997));
#14249=CARTESIAN_POINT('Ctrl Pts',(-0.0266020595922903,8.39,7.605));
#14250=CARTESIAN_POINT('Ctrl Pts',(0.0266020595922903,8.39,7.605));
#14251=CARTESIAN_POINT('Ctrl Pts',(0.0548298721325189,8.39536143894557,
7.6030741628997));
#14252=CARTESIAN_POINT('Ctrl Pts',(0.100109787682299,8.41420068341256,7.59698224789957));
#14253=CARTESIAN_POINT('Ctrl Pts',(0.1182543952608,8.42527883178237,7.59354677224418));
#14254=CARTESIAN_POINT('Ctrl Pts',(0.133884278389956,8.43821310312636,7.59));
#14255=CARTESIAN_POINT('',(-0.21,8.6,7.59));
#14256=CARTESIAN_POINT('Origin',(0.,8.6,7.59));
#14257=CARTESIAN_POINT('',(-0.21,8.6,7.97770138590472));
#14258=CARTESIAN_POINT('',(-0.21,8.6,7.59));
#14259=CARTESIAN_POINT('',(0.21,8.6,7.97770138590472));
#14260=CARTESIAN_POINT('Ctrl Pts',(0.21,8.6,7.97770138590472));
#14261=CARTESIAN_POINT('Ctrl Pts',(0.21,8.57354611741017,7.97770138590472));
#14262=CARTESIAN_POINT('Ctrl Pts',(0.204697017125528,8.54538474169131,7.97888646613217));
#14263=CARTESIAN_POINT('Ctrl Pts',(0.183241751515529,8.49366957869826,7.98312869991148));
#14264=CARTESIAN_POINT('Ctrl Pts',(0.167093586802906,8.47010873870456,7.98612044796649));
#14265=CARTESIAN_POINT('Ctrl Pts',(0.129892533236543,8.43290768513819,7.99170645156379));
#14266=CARTESIAN_POINT('Ctrl Pts',(0.106331154992714,8.41675852489431,7.99466914446598));
#14267=CARTESIAN_POINT('Ctrl Pts',(0.0546141143983522,8.39530253627557,
7.99884449237241));
#14268=CARTESIAN_POINT('Ctrl Pts',(0.0264520736824499,8.39,8.));
#14269=CARTESIAN_POINT('Ctrl Pts',(-0.0264520736824498,8.39,8.));
#14270=CARTESIAN_POINT('Ctrl Pts',(-0.0546141143983521,8.39530253627557,
7.99884449237241));
#14271=CARTESIAN_POINT('Ctrl Pts',(-0.106331154992714,8.41675852489431,
7.99466914446598));
#14272=CARTESIAN_POINT('Ctrl Pts',(-0.129892533236543,8.43290768513819,
7.99170645156379));
#14273=CARTESIAN_POINT('Ctrl Pts',(-0.167093586802906,8.47010873870456,
7.98612044796649));
#14274=CARTESIAN_POINT('Ctrl Pts',(-0.183241751515529,8.49366957869826,
7.98312869991148));
#14275=CARTESIAN_POINT('Ctrl Pts',(-0.204697017125528,8.54538474169131,
7.97888646613217));
#14276=CARTESIAN_POINT('Ctrl Pts',(-0.21,8.57354611741017,7.97770138590472));
#14277=CARTESIAN_POINT('Ctrl Pts',(-0.21,8.6,7.97770138590472));
#14278=CARTESIAN_POINT('Ctrl Pts',(-0.21,8.6,7.97770138590472));
#14279=CARTESIAN_POINT('Ctrl Pts',(-0.21,8.62645388258982,7.97770138590472));
#14280=CARTESIAN_POINT('Ctrl Pts',(-0.204697017125528,8.65461525830868,
7.97888646613217));
#14281=CARTESIAN_POINT('Ctrl Pts',(-0.183241751515529,8.70633042130174,
7.98312869991148));
#14282=CARTESIAN_POINT('Ctrl Pts',(-0.167093586802906,8.72989126129544,
7.98612044796649));
#14283=CARTESIAN_POINT('Ctrl Pts',(-0.129892533236543,8.76709231486181,
7.99170645156379));
#14284=CARTESIAN_POINT('Ctrl Pts',(-0.106331154992714,8.78324147510569,
7.99466914446598));
#14285=CARTESIAN_POINT('Ctrl Pts',(-0.0546141143983522,8.80469746372443,
7.99884449237241));
#14286=CARTESIAN_POINT('Ctrl Pts',(-0.0264520736824499,8.81,8.));
#14287=CARTESIAN_POINT('Ctrl Pts',(0.0264520736824499,8.81,8.));
#14288=CARTESIAN_POINT('Ctrl Pts',(0.0546141143983521,8.80469746372443,
7.99884449237241));
#14289=CARTESIAN_POINT('Ctrl Pts',(0.106331154992713,8.78324147510569,7.99466914446598));
#14290=CARTESIAN_POINT('Ctrl Pts',(0.129892533236543,8.76709231486181,7.99170645156379));
#14291=CARTESIAN_POINT('Ctrl Pts',(0.167093586802906,8.72989126129544,7.98612044796649));
#14292=CARTESIAN_POINT('Ctrl Pts',(0.183241751515529,8.70633042130174,7.98312869991148));
#14293=CARTESIAN_POINT('Ctrl Pts',(0.204697017125528,8.65461525830868,7.97888646613217));
#14294=CARTESIAN_POINT('Ctrl Pts',(0.21,8.62645388258982,7.97770138590472));
#14295=CARTESIAN_POINT('Ctrl Pts',(0.21,8.6,7.97770138590472));
#14296=CARTESIAN_POINT('',(-0.133884278389956,8.76178689687364,7.59));
#14297=CARTESIAN_POINT('Origin',(0.,8.6,7.59));
#14298=CARTESIAN_POINT('Ctrl Pts',(0.133884278389955,8.76178689687364,7.59));
#14299=CARTESIAN_POINT('Ctrl Pts',(0.1182543952608,8.77472116821763,7.59354677224418));
#14300=CARTESIAN_POINT('Ctrl Pts',(0.100109787682298,8.78579931658744,7.59698224789957));
#14301=CARTESIAN_POINT('Ctrl Pts',(0.054829872132519,8.80463856105443,7.6030741628997));
#14302=CARTESIAN_POINT('Ctrl Pts',(0.0266020595922903,8.81,7.605));
#14303=CARTESIAN_POINT('Ctrl Pts',(-0.0266020595922903,8.81,7.605));
#14304=CARTESIAN_POINT('Ctrl Pts',(-0.0548298721325189,8.80463856105443,
7.6030741628997));
#14305=CARTESIAN_POINT('Ctrl Pts',(-0.100109787682299,8.78579931658744,
7.59698224789957));
#14306=CARTESIAN_POINT('Ctrl Pts',(-0.118254395260801,8.77472116821763,
7.59354677224418));
#14307=CARTESIAN_POINT('Ctrl Pts',(-0.133884278389955,8.76178689687364,
7.59));
#14308=CARTESIAN_POINT('Origin',(0.,8.6,7.59));
#14309=CARTESIAN_POINT('',(-0.133884278389956,8.2,7.59));
#14310=CARTESIAN_POINT('Origin',(0.,8.2,7.));
#14311=CARTESIAN_POINT('',(-0.605,9.,7.));
#14312=CARTESIAN_POINT('Origin',(0.,9.,7.));
#14313=CARTESIAN_POINT('',(-0.605,8.2,7.));
#14314=CARTESIAN_POINT('',(-0.605,8.2,7.));
#14315=CARTESIAN_POINT('Origin',(0.,8.2,7.));
#14316=CARTESIAN_POINT('Origin',(0.,8.2,7.));
#14317=CARTESIAN_POINT('',(-1.,9.,7.));
#14318=CARTESIAN_POINT('Origin',(0.,9.,7.));
#14319=CARTESIAN_POINT('',(-1.,8.2,7.));
#14320=CARTESIAN_POINT('',(-1.,8.2,7.));
#14321=CARTESIAN_POINT('Origin',(0.,8.2,7.));
#14322=CARTESIAN_POINT('Origin',(0.,9.,7.));
#14323=CARTESIAN_POINT('Origin',(0.,8.2,7.));
#14324=CARTESIAN_POINT('',(0.,0.,0.));
#14325=CARTESIAN_POINT('Origin',(0.,-8.2,7.));
#14326=CARTESIAN_POINT('',(-0.605,-7.5,7.));
#14327=CARTESIAN_POINT('Origin',(0.,-7.5,7.));
#14328=CARTESIAN_POINT('',(-0.605,-8.2,7.));
#14329=CARTESIAN_POINT('',(-0.605,-8.2,7.));
#14330=CARTESIAN_POINT('Origin',(0.,-8.2,7.));
#14331=CARTESIAN_POINT('Origin',(0.,-8.2,7.));
#14332=CARTESIAN_POINT('',(-0.9,-7.5,7.));
#14333=CARTESIAN_POINT('Origin',(0.,-7.5,7.));
#14334=CARTESIAN_POINT('',(-0.9,-8.2,7.));
#14335=CARTESIAN_POINT('',(-0.9,-8.2,7.));
#14336=CARTESIAN_POINT('Origin',(0.,-8.2,7.));
#14337=CARTESIAN_POINT('Origin',(0.,-7.5,7.));
#14338=CARTESIAN_POINT('Origin',(0.,-8.2,7.));
#14339=CARTESIAN_POINT('',(0.,0.,0.));
#14340=CARTESIAN_POINT('Origin',(0.,7.5,7.));
#14341=CARTESIAN_POINT('',(-0.605,8.2,7.));
#14342=CARTESIAN_POINT('Origin',(0.,8.2,7.));
#14343=CARTESIAN_POINT('',(-0.605,7.5,7.));
#14344=CARTESIAN_POINT('',(-0.605,7.5,7.));
#14345=CARTESIAN_POINT('Origin',(0.,7.5,7.));
#14346=CARTESIAN_POINT('Origin',(0.,7.5,7.));
#14347=CARTESIAN_POINT('',(-0.9,8.2,7.));
#14348=CARTESIAN_POINT('Origin',(0.,8.2,7.));
#14349=CARTESIAN_POINT('',(-0.9,7.5,7.));
#14350=CARTESIAN_POINT('',(-0.9,7.5,7.));
#14351=CARTESIAN_POINT('Origin',(0.,7.5,7.));
#14352=CARTESIAN_POINT('Origin',(0.,8.2,7.));
#14353=CARTESIAN_POINT('Origin',(0.,7.5,7.));
#14354=CARTESIAN_POINT('',(0.,0.,0.));
#14355=CARTESIAN_POINT('Origin',(0.,-1.1,7.99));
#14356=CARTESIAN_POINT('',(0.172988438920056,-1.21905880899792,7.99));
#14357=CARTESIAN_POINT('',(0.172988438920056,-0.980941191002085,7.99));
#14358=CARTESIAN_POINT('',(0.172988438920056,-1.5,7.99));
#14359=CARTESIAN_POINT('Origin',(0.,-1.1,7.99));
#14360=CARTESIAN_POINT('Origin',(0.,-1.1,7.99));
#14361=CARTESIAN_POINT('',(-0.172988438920056,-1.21905880899792,7.99));
#14362=CARTESIAN_POINT('Ctrl Pts',(-0.172988438920056,-1.21905880899792,
7.99));
#14363=CARTESIAN_POINT('Ctrl Pts',(-0.165594865311315,-1.22980142239529,
7.99129192197638));
#14364=CARTESIAN_POINT('Ctrl Pts',(-0.157297138725606,-1.23968770937274,
7.99265394943905));
#14365=CARTESIAN_POINT('Ctrl Pts',(-0.129892073845076,-1.26709277425327,
7.9967480843909));
#14366=CARTESIAN_POINT('Ctrl Pts',(-0.106330167759285,-1.28324205633295,
7.99969589327638));
#14367=CARTESIAN_POINT('Ctrl Pts',(-0.0546129046324105,-1.30469779396491,
8.00385029472357));
#14368=CARTESIAN_POINT('Ctrl Pts',(-0.0264512308298516,-1.31,8.005));
#14369=CARTESIAN_POINT('Ctrl Pts',(0.0264512308298515,-1.31,8.005));
#14370=CARTESIAN_POINT('Ctrl Pts',(0.0546129046324104,-1.30469779396491,
8.00385029472357));
#14371=CARTESIAN_POINT('Ctrl Pts',(0.106330167759284,-1.28324205633295,
7.99969589327638));
#14372=CARTESIAN_POINT('Ctrl Pts',(0.129892073845076,-1.26709277425327,
7.9967480843909));
#14373=CARTESIAN_POINT('Ctrl Pts',(0.157297138725606,-1.23968770937274,
7.99265394943905));
#14374=CARTESIAN_POINT('Ctrl Pts',(0.165594865311314,-1.22980142239529,
7.99129192197638));
#14375=CARTESIAN_POINT('Ctrl Pts',(0.172988438920056,-1.21905880899792,
7.99));
#14376=CARTESIAN_POINT('',(-0.21,-1.1,7.99));
#14377=CARTESIAN_POINT('Origin',(0.,-1.1,7.99));
#14378=CARTESIAN_POINT('',(-0.21,-1.1,8.48522725533839));
#14379=CARTESIAN_POINT('',(-0.21,-1.1,7.99));
#14380=CARTESIAN_POINT('',(0.21,-1.1,8.48522725533839));
#14381=CARTESIAN_POINT('Ctrl Pts',(0.21,-1.1,8.48522725533839));
#14382=CARTESIAN_POINT('Ctrl Pts',(0.21,-1.12640552692445,8.48522725533839));
#14383=CARTESIAN_POINT('Ctrl Pts',(0.204715737269596,-1.15454707409071,
8.48600415954412));
#14384=CARTESIAN_POINT('Ctrl Pts',(0.183273763036331,-1.20627626890513,
8.48880073282317));
#14385=CARTESIAN_POINT('Ctrl Pts',(0.167117923970394,-1.22986692412796,
8.49077897157582));
#14386=CARTESIAN_POINT('Ctrl Pts',(0.129867169887369,-1.26711767821098,
8.49448481141327));
#14387=CARTESIAN_POINT('Ctrl Pts',(0.106276408305765,-1.28327371000135,
8.49645455657129));
#14388=CARTESIAN_POINT('Ctrl Pts',(0.0545468514059002,-1.30471582482622,
8.49923165515646));
#14389=CARTESIAN_POINT('Ctrl Pts',(0.0264051785092814,-1.31,8.5));
#14390=CARTESIAN_POINT('Ctrl Pts',(-0.0264051785092814,-1.31,8.5));
#14391=CARTESIAN_POINT('Ctrl Pts',(-0.0545468514059001,-1.30471582482622,
8.49923165515646));
#14392=CARTESIAN_POINT('Ctrl Pts',(-0.106276408305765,-1.28327371000135,
8.49645455657129));
#14393=CARTESIAN_POINT('Ctrl Pts',(-0.129867169887369,-1.26711767821098,
8.49448481141327));
#14394=CARTESIAN_POINT('Ctrl Pts',(-0.167117923970394,-1.22986692412796,
8.49077897157582));
#14395=CARTESIAN_POINT('Ctrl Pts',(-0.183273763036331,-1.20627626890513,
8.48880073282317));
#14396=CARTESIAN_POINT('Ctrl Pts',(-0.204715737269596,-1.15454707409071,
8.48600415954412));
#14397=CARTESIAN_POINT('Ctrl Pts',(-0.21,-1.12640552692445,8.48522725533839));
#14398=CARTESIAN_POINT('Ctrl Pts',(-0.21,-1.1,8.48522725533839));
#14399=CARTESIAN_POINT('Ctrl Pts',(-0.21,-1.1,8.48522725533839));
#14400=CARTESIAN_POINT('Ctrl Pts',(-0.21,-1.07359447307555,8.48522725533839));
#14401=CARTESIAN_POINT('Ctrl Pts',(-0.204715737269596,-1.04545292590929,
8.48600415954412));
#14402=CARTESIAN_POINT('Ctrl Pts',(-0.183273763036331,-0.993723731094873,
8.48880073282317));
#14403=CARTESIAN_POINT('Ctrl Pts',(-0.167117923970394,-0.970133075872044,
8.49077897157582));
#14404=CARTESIAN_POINT('Ctrl Pts',(-0.129867169887369,-0.932882321789019,
8.49448481141327));
#14405=CARTESIAN_POINT('Ctrl Pts',(-0.106276408305765,-0.916726289998648,
8.49645455657129));
#14406=CARTESIAN_POINT('Ctrl Pts',(-0.0545468514059001,-0.895284175173782,
8.49923165515646));
#14407=CARTESIAN_POINT('Ctrl Pts',(-0.0264051785092814,-0.89,8.5));
#14408=CARTESIAN_POINT('Ctrl Pts',(0.0264051785092814,-0.89,8.5));
#14409=CARTESIAN_POINT('Ctrl Pts',(0.0545468514059001,-0.895284175173782,
8.49923165515645));
#14410=CARTESIAN_POINT('Ctrl Pts',(0.106276408305765,-0.916726289998648,
8.49645455657129));
#14411=CARTESIAN_POINT('Ctrl Pts',(0.129867169887369,-0.932882321789019,
8.49448481141327));
#14412=CARTESIAN_POINT('Ctrl Pts',(0.167117923970394,-0.970133075872044,
8.49077897157582));
#14413=CARTESIAN_POINT('Ctrl Pts',(0.183273763036331,-0.993723731094873,
8.48880073282317));
#14414=CARTESIAN_POINT('Ctrl Pts',(0.204715737269596,-1.04545292590929,
8.48600415954412));
#14415=CARTESIAN_POINT('Ctrl Pts',(0.21,-1.07359447307555,8.48522725533839));
#14416=CARTESIAN_POINT('Ctrl Pts',(0.21,-1.1,8.48522725533839));
#14417=CARTESIAN_POINT('',(-0.172988438920056,-0.980941191002085,7.99));
#14418=CARTESIAN_POINT('Origin',(0.,-1.1,7.99));
#14419=CARTESIAN_POINT('Ctrl Pts',(0.172988438920056,-0.980941191002085,
7.99));
#14420=CARTESIAN_POINT('Ctrl Pts',(0.165594865311315,-0.970198577604708,
7.99129192197638));
#14421=CARTESIAN_POINT('Ctrl Pts',(0.157297138725606,-0.960312290627256,
7.99265394943905));
#14422=CARTESIAN_POINT('Ctrl Pts',(0.129892073845076,-0.932907225746726,
7.9967480843909));
#14423=CARTESIAN_POINT('Ctrl Pts',(0.106330167759284,-0.916757943667051,
7.99969589327638));
#14424=CARTESIAN_POINT('Ctrl Pts',(0.0546129046324105,-0.895302206035094,
8.00385029472357));
#14425=CARTESIAN_POINT('Ctrl Pts',(0.0264512308298516,-0.89,8.005));
#14426=CARTESIAN_POINT('Ctrl Pts',(-0.0264512308298516,-0.89,8.005));
#14427=CARTESIAN_POINT('Ctrl Pts',(-0.0546129046324105,-0.895302206035094,
8.00385029472357));
#14428=CARTESIAN_POINT('Ctrl Pts',(-0.106330167759284,-0.916757943667051,
7.99969589327638));
#14429=CARTESIAN_POINT('Ctrl Pts',(-0.129892073845076,-0.932907225746726,
7.9967480843909));
#14430=CARTESIAN_POINT('Ctrl Pts',(-0.157297138725606,-0.960312290627256,
7.99265394943905));
#14431=CARTESIAN_POINT('Ctrl Pts',(-0.165594865311314,-0.970198577604708,
7.99129192197638));
#14432=CARTESIAN_POINT('Ctrl Pts',(-0.172988438920056,-0.980941191002085,
7.99));
#14433=CARTESIAN_POINT('Origin',(0.,-1.1,7.99));
#14434=CARTESIAN_POINT('',(-0.172988438920056,-1.5,7.99));
#14435=CARTESIAN_POINT('Origin',(0.,-1.5,7.));
#14436=CARTESIAN_POINT('',(-1.005,-0.7,7.));
#14437=CARTESIAN_POINT('Origin',(0.,-0.7,7.));
#14438=CARTESIAN_POINT('',(-1.005,-1.5,7.));
#14439=CARTESIAN_POINT('',(-1.005,-1.5,7.));
#14440=CARTESIAN_POINT('Origin',(0.,-1.5,7.));
#14441=CARTESIAN_POINT('Origin',(0.,-1.5,7.));
#14442=CARTESIAN_POINT('',(-1.5,-0.7,7.));
#14443=CARTESIAN_POINT('Origin',(0.,-0.7,7.));
#14444=CARTESIAN_POINT('',(-1.5,-1.5,7.));
#14445=CARTESIAN_POINT('',(-1.5,-1.5,7.));
#14446=CARTESIAN_POINT('Origin',(0.,-1.5,7.));
#14447=CARTESIAN_POINT('Origin',(0.,-0.7,7.));
#14448=CARTESIAN_POINT('Origin',(0.,-1.5,7.));
#14449=CARTESIAN_POINT('',(0.,0.,0.));
#14450=CARTESIAN_POINT('Origin',(0.,1.1,7.99));
#14451=CARTESIAN_POINT('',(0.172988438920056,0.980941191002085,7.99));
#14452=CARTESIAN_POINT('',(0.172988438920056,1.21905880899792,7.99));
#14453=CARTESIAN_POINT('',(0.172988438920056,0.7,7.99));
#14454=CARTESIAN_POINT('Origin',(0.,1.1,7.99));
#14455=CARTESIAN_POINT('Origin',(0.,1.1,7.99));
#14456=CARTESIAN_POINT('',(-0.172988438920056,0.980941191002085,7.99));
#14457=CARTESIAN_POINT('Ctrl Pts',(-0.172988438920056,0.980941191002085,
7.99));
#14458=CARTESIAN_POINT('Ctrl Pts',(-0.165594865311315,0.970198577604708,
7.99129192197638));
#14459=CARTESIAN_POINT('Ctrl Pts',(-0.157297138725606,0.960312290627256,
7.99265394943905));
#14460=CARTESIAN_POINT('Ctrl Pts',(-0.129892073845076,0.932907225746726,
7.9967480843909));
#14461=CARTESIAN_POINT('Ctrl Pts',(-0.106330167759285,0.916757943667051,
7.99969589327638));
#14462=CARTESIAN_POINT('Ctrl Pts',(-0.0546129046324106,0.895302206035095,
8.00385029472357));
#14463=CARTESIAN_POINT('Ctrl Pts',(-0.0264512308298516,0.89,8.005));
#14464=CARTESIAN_POINT('Ctrl Pts',(0.0264512308298515,0.89,8.005));
#14465=CARTESIAN_POINT('Ctrl Pts',(0.0546129046324105,0.895302206035094,
8.00385029472357));
#14466=CARTESIAN_POINT('Ctrl Pts',(0.106330167759284,0.916757943667051,
7.99969589327638));
#14467=CARTESIAN_POINT('Ctrl Pts',(0.129892073845076,0.932907225746726,
7.9967480843909));
#14468=CARTESIAN_POINT('Ctrl Pts',(0.157297138725606,0.960312290627256,
7.99265394943905));
#14469=CARTESIAN_POINT('Ctrl Pts',(0.165594865311314,0.970198577604708,
7.99129192197638));
#14470=CARTESIAN_POINT('Ctrl Pts',(0.172988438920056,0.980941191002085,
7.99));
#14471=CARTESIAN_POINT('',(-0.21,1.1,7.99));
#14472=CARTESIAN_POINT('Origin',(0.,1.1,7.99));
#14473=CARTESIAN_POINT('',(-0.21,1.1,8.48522725533839));
#14474=CARTESIAN_POINT('',(-0.21,1.1,7.99));
#14475=CARTESIAN_POINT('',(0.21,1.1,8.48522725533839));
#14476=CARTESIAN_POINT('Ctrl Pts',(0.21,1.1,8.48522725533839));
#14477=CARTESIAN_POINT('Ctrl Pts',(0.21,1.07359447307555,8.48522725533839));
#14478=CARTESIAN_POINT('Ctrl Pts',(0.204715737269596,1.04545292590929,8.48600415954412));
#14479=CARTESIAN_POINT('Ctrl Pts',(0.183273763036331,0.993723731094873,
8.48880073282317));
#14480=CARTESIAN_POINT('Ctrl Pts',(0.167117923970394,0.970133075872044,
8.49077897157582));
#14481=CARTESIAN_POINT('Ctrl Pts',(0.129867169887369,0.932882321789019,
8.49448481141327));
#14482=CARTESIAN_POINT('Ctrl Pts',(0.106276408305765,0.916726289998648,
8.49645455657129));
#14483=CARTESIAN_POINT('Ctrl Pts',(0.0545468514059001,0.895284175173782,
8.49923165515646));
#14484=CARTESIAN_POINT('Ctrl Pts',(0.0264051785092814,0.89,8.5));
#14485=CARTESIAN_POINT('Ctrl Pts',(-0.0264051785092814,0.89,8.5));
#14486=CARTESIAN_POINT('Ctrl Pts',(-0.0545468514059001,0.895284175173782,
8.49923165515646));
#14487=CARTESIAN_POINT('Ctrl Pts',(-0.106276408305765,0.916726289998648,
8.49645455657129));
#14488=CARTESIAN_POINT('Ctrl Pts',(-0.129867169887369,0.932882321789019,
8.49448481141327));
#14489=CARTESIAN_POINT('Ctrl Pts',(-0.167117923970394,0.970133075872044,
8.49077897157582));
#14490=CARTESIAN_POINT('Ctrl Pts',(-0.183273763036331,0.993723731094873,
8.48880073282317));
#14491=CARTESIAN_POINT('Ctrl Pts',(-0.204715737269596,1.04545292590929,
8.48600415954412));
#14492=CARTESIAN_POINT('Ctrl Pts',(-0.21,1.07359447307555,8.48522725533839));
#14493=CARTESIAN_POINT('Ctrl Pts',(-0.21,1.1,8.48522725533839));
#14494=CARTESIAN_POINT('Ctrl Pts',(-0.21,1.1,8.48522725533839));
#14495=CARTESIAN_POINT('Ctrl Pts',(-0.21,1.12640552692445,8.48522725533839));
#14496=CARTESIAN_POINT('Ctrl Pts',(-0.204715737269596,1.15454707409071,
8.48600415954412));
#14497=CARTESIAN_POINT('Ctrl Pts',(-0.183273763036331,1.20627626890513,
8.48880073282317));
#14498=CARTESIAN_POINT('Ctrl Pts',(-0.167117923970394,1.22986692412796,
8.49077897157582));
#14499=CARTESIAN_POINT('Ctrl Pts',(-0.129867169887369,1.26711767821098,
8.49448481141327));
#14500=CARTESIAN_POINT('Ctrl Pts',(-0.106276408305765,1.28327371000135,
8.49645455657129));
#14501=CARTESIAN_POINT('Ctrl Pts',(-0.0545468514059002,1.30471582482622,
8.49923165515646));
#14502=CARTESIAN_POINT('Ctrl Pts',(-0.0264051785092814,1.31,8.5));
#14503=CARTESIAN_POINT('Ctrl Pts',(0.0264051785092814,1.31,8.5));
#14504=CARTESIAN_POINT('Ctrl Pts',(0.0545468514059003,1.30471582482622,
8.49923165515645));
#14505=CARTESIAN_POINT('Ctrl Pts',(0.106276408305765,1.28327371000135,8.49645455657129));
#14506=CARTESIAN_POINT('Ctrl Pts',(0.129867169887369,1.26711767821098,8.49448481141327));
#14507=CARTESIAN_POINT('Ctrl Pts',(0.167117923970394,1.22986692412796,8.49077897157582));
#14508=CARTESIAN_POINT('Ctrl Pts',(0.183273763036332,1.20627626890513,8.48880073282317));
#14509=CARTESIAN_POINT('Ctrl Pts',(0.204715737269596,1.15454707409071,8.48600415954412));
#14510=CARTESIAN_POINT('Ctrl Pts',(0.21,1.12640552692445,8.48522725533839));
#14511=CARTESIAN_POINT('Ctrl Pts',(0.21,1.1,8.48522725533839));
#14512=CARTESIAN_POINT('',(-0.172988438920056,1.21905880899792,7.99));
#14513=CARTESIAN_POINT('Origin',(0.,1.1,7.99));
#14514=CARTESIAN_POINT('Ctrl Pts',(0.172988438920056,1.21905880899792,7.99));
#14515=CARTESIAN_POINT('Ctrl Pts',(0.165594865311314,1.22980142239529,7.99129192197638));
#14516=CARTESIAN_POINT('Ctrl Pts',(0.157297138725606,1.23968770937274,7.99265394943905));
#14517=CARTESIAN_POINT('Ctrl Pts',(0.129892073845076,1.26709277425327,7.9967480843909));
#14518=CARTESIAN_POINT('Ctrl Pts',(0.106330167759284,1.28324205633295,7.99969589327638));
#14519=CARTESIAN_POINT('Ctrl Pts',(0.0546129046324105,1.30469779396491,
8.00385029472357));
#14520=CARTESIAN_POINT('Ctrl Pts',(0.0264512308298516,1.31,8.005));
#14521=CARTESIAN_POINT('Ctrl Pts',(-0.0264512308298516,1.31,8.005));
#14522=CARTESIAN_POINT('Ctrl Pts',(-0.0546129046324105,1.30469779396491,
8.00385029472357));
#14523=CARTESIAN_POINT('Ctrl Pts',(-0.106330167759284,1.28324205633295,
7.99969589327638));
#14524=CARTESIAN_POINT('Ctrl Pts',(-0.129892073845076,1.26709277425327,
7.9967480843909));
#14525=CARTESIAN_POINT('Ctrl Pts',(-0.157297138725606,1.23968770937274,
7.99265394943905));
#14526=CARTESIAN_POINT('Ctrl Pts',(-0.165594865311314,1.22980142239529,
7.99129192197638));
#14527=CARTESIAN_POINT('Ctrl Pts',(-0.172988438920056,1.21905880899792,
7.99));
#14528=CARTESIAN_POINT('Origin',(0.,1.1,7.99));
#14529=CARTESIAN_POINT('',(-0.172988438920056,0.7,7.99));
#14530=CARTESIAN_POINT('Origin',(0.,0.7,7.));
#14531=CARTESIAN_POINT('',(-1.005,1.5,7.));
#14532=CARTESIAN_POINT('Origin',(0.,1.5,7.));
#14533=CARTESIAN_POINT('',(-1.005,0.7,7.));
#14534=CARTESIAN_POINT('',(-1.005,0.7,7.));
#14535=CARTESIAN_POINT('Origin',(0.,0.7,7.));
#14536=CARTESIAN_POINT('Origin',(0.,0.7,7.));
#14537=CARTESIAN_POINT('',(-1.5,1.5,7.));
#14538=CARTESIAN_POINT('Origin',(0.,1.5,7.));
#14539=CARTESIAN_POINT('',(-1.5,0.7,7.));
#14540=CARTESIAN_POINT('',(-1.5,0.7,7.));
#14541=CARTESIAN_POINT('Origin',(0.,0.7,7.));
#14542=CARTESIAN_POINT('Origin',(0.,1.5,7.));
#14543=CARTESIAN_POINT('Origin',(0.,0.7,7.));
#14544=CARTESIAN_POINT('',(0.,0.,0.));
#14545=CARTESIAN_POINT('Origin',(0.,-9.8,7.59));
#14546=CARTESIAN_POINT('',(0.109087121146353,-9.97944358444927,7.59));
#14547=CARTESIAN_POINT('',(0.109087121146353,-9.62055641555073,7.59));
#14548=CARTESIAN_POINT('',(0.109087121146353,-11.,7.59));
#14549=CARTESIAN_POINT('Origin',(0.,-9.8,7.59));
#14550=CARTESIAN_POINT('Origin',(0.,-9.8,7.59));
#14551=CARTESIAN_POINT('',(-0.109087121146353,-9.97944358444927,7.59));
#14552=CARTESIAN_POINT('Ctrl Pts',(-0.109087121146354,-9.97944358444927,
7.59));
#14553=CARTESIAN_POINT('Ctrl Pts',(-0.100058962329431,-9.98493197155217,
7.59166924721117));
#14554=CARTESIAN_POINT('Ctrl Pts',(-0.0905297208284648,-9.98978489888129,
7.59321436338553));
#14555=CARTESIAN_POINT('Ctrl Pts',(-0.0548356965671429,-10.0046369707595,
7.598057680137));
#14556=CARTESIAN_POINT('Ctrl Pts',(-0.026606099485122,-10.01,7.6));
#14557=CARTESIAN_POINT('Ctrl Pts',(0.0266060994851219,-10.01,7.6));
#14558=CARTESIAN_POINT('Ctrl Pts',(0.0548356965671429,-10.0046369707595,
7.598057680137));
#14559=CARTESIAN_POINT('Ctrl Pts',(0.0905297208284645,-9.98978489888129,
7.59321436338553));
#14560=CARTESIAN_POINT('Ctrl Pts',(0.100058962329432,-9.98493197155217,
7.59166924721117));
#14561=CARTESIAN_POINT('Ctrl Pts',(0.109087121146353,-9.97944358444927,
7.59));
#14562=CARTESIAN_POINT('',(-0.21,-9.8,7.59));
#14563=CARTESIAN_POINT('Origin',(0.,-9.8,7.59));
#14564=CARTESIAN_POINT('',(-0.21,-9.8,8.48522725533839));
#14565=CARTESIAN_POINT('',(-0.21,-9.8,7.59));
#14566=CARTESIAN_POINT('',(0.21,-9.8,8.48522725533839));
#14567=CARTESIAN_POINT('Ctrl Pts',(0.21,-9.8,8.48522725533839));
#14568=CARTESIAN_POINT('Ctrl Pts',(0.21,-9.82640552692446,8.48522725533839));
#14569=CARTESIAN_POINT('Ctrl Pts',(0.204715737269595,-9.85454707409072,
8.48600415954412));
#14570=CARTESIAN_POINT('Ctrl Pts',(0.183273763036331,-9.90627626890513,
8.48880073282317));
#14571=CARTESIAN_POINT('Ctrl Pts',(0.167117923970394,-9.92986692412796,
8.49077897157582));
#14572=CARTESIAN_POINT('Ctrl Pts',(0.129867169887369,-9.96711767821098,
8.49448481141327));
#14573=CARTESIAN_POINT('Ctrl Pts',(0.106276408305765,-9.98327371000135,
8.49645455657129));
#14574=CARTESIAN_POINT('Ctrl Pts',(0.0545468514059001,-10.0047158248262,
8.49923165515646));
#14575=CARTESIAN_POINT('Ctrl Pts',(0.0264051785092814,-10.01,8.5));
#14576=CARTESIAN_POINT('Ctrl Pts',(-0.0264051785092814,-10.01,8.5));
#14577=CARTESIAN_POINT('Ctrl Pts',(-0.0545468514058994,-10.0047158248262,
8.49923165515646));
#14578=CARTESIAN_POINT('Ctrl Pts',(-0.106276408305765,-9.98327371000135,
8.49645455657129));
#14579=CARTESIAN_POINT('Ctrl Pts',(-0.129867169887368,-9.96711767821098,
8.49448481141327));
#14580=CARTESIAN_POINT('Ctrl Pts',(-0.167117923970393,-9.92986692412796,
8.49077897157582));
#14581=CARTESIAN_POINT('Ctrl Pts',(-0.183273763036331,-9.90627626890513,
8.48880073282317));
#14582=CARTESIAN_POINT('Ctrl Pts',(-0.204715737269595,-9.85454707409072,
8.48600415954412));
#14583=CARTESIAN_POINT('Ctrl Pts',(-0.21,-9.82640552692446,8.48522725533839));
#14584=CARTESIAN_POINT('Ctrl Pts',(-0.21,-9.8,8.48522725533839));
#14585=CARTESIAN_POINT('Ctrl Pts',(-0.21,-9.8,8.48522725533839));
#14586=CARTESIAN_POINT('Ctrl Pts',(-0.21,-9.77359447307554,8.48522725533839));
#14587=CARTESIAN_POINT('Ctrl Pts',(-0.204715737269595,-9.74545292590929,
8.48600415954412));
#14588=CARTESIAN_POINT('Ctrl Pts',(-0.183273763036331,-9.69372373109487,
8.48880073282317));
#14589=CARTESIAN_POINT('Ctrl Pts',(-0.167117923970394,-9.67013307587204,
8.49077897157582));
#14590=CARTESIAN_POINT('Ctrl Pts',(-0.129867169887369,-9.63288232178902,
8.49448481141327));
#14591=CARTESIAN_POINT('Ctrl Pts',(-0.106276408305765,-9.61672628999865,
8.49645455657129));
#14592=CARTESIAN_POINT('Ctrl Pts',(-0.0545468514059001,-9.59528417517378,
8.49923165515646));
#14593=CARTESIAN_POINT('Ctrl Pts',(-0.0264051785092815,-9.59,8.5));
#14594=CARTESIAN_POINT('Ctrl Pts',(0.0264051785092813,-9.59,8.5));
#14595=CARTESIAN_POINT('Ctrl Pts',(0.0545468514058994,-9.59528417517378,
8.49923165515645));
#14596=CARTESIAN_POINT('Ctrl Pts',(0.106276408305765,-9.61672628999865,
8.49645455657129));
#14597=CARTESIAN_POINT('Ctrl Pts',(0.129867169887368,-9.63288232178902,
8.49448481141327));
#14598=CARTESIAN_POINT('Ctrl Pts',(0.167117923970393,-9.67013307587204,
8.49077897157582));
#14599=CARTESIAN_POINT('Ctrl Pts',(0.183273763036331,-9.69372373109487,
8.48880073282317));
#14600=CARTESIAN_POINT('Ctrl Pts',(0.204715737269595,-9.74545292590929,
8.48600415954412));
#14601=CARTESIAN_POINT('Ctrl Pts',(0.21,-9.77359447307554,8.48522725533839));
#14602=CARTESIAN_POINT('Ctrl Pts',(0.21,-9.8,8.48522725533839));
#14603=CARTESIAN_POINT('',(-0.109087121146353,-9.62055641555073,7.59));
#14604=CARTESIAN_POINT('Origin',(0.,-9.8,7.59));
#14605=CARTESIAN_POINT('Ctrl Pts',(0.109087121146353,-9.62055641555074,
7.59));
#14606=CARTESIAN_POINT('Ctrl Pts',(0.100058962329431,-9.61506802844783,
7.59166924721117));
#14607=CARTESIAN_POINT('Ctrl Pts',(0.0905297208284649,-9.61021510111872,
7.59321436338553));
#14608=CARTESIAN_POINT('Ctrl Pts',(0.054835696567143,-9.59536302924048,
7.598057680137));
#14609=CARTESIAN_POINT('Ctrl Pts',(0.026606099485122,-9.59,7.6));
#14610=CARTESIAN_POINT('Ctrl Pts',(-0.026606099485122,-9.59,7.6));
#14611=CARTESIAN_POINT('Ctrl Pts',(-0.0548356965671429,-9.59536302924048,
7.598057680137));
#14612=CARTESIAN_POINT('Ctrl Pts',(-0.090529720828465,-9.61021510111872,
7.59321436338553));
#14613=CARTESIAN_POINT('Ctrl Pts',(-0.100058962329431,-9.61506802844783,
7.59166924721117));
#14614=CARTESIAN_POINT('Ctrl Pts',(-0.109087121146353,-9.62055641555073,
7.59));
#14615=CARTESIAN_POINT('Origin',(0.,-9.8,7.59));
#14616=CARTESIAN_POINT('',(-0.109087121146353,-11.,7.59));
#14617=CARTESIAN_POINT('Origin',(-1.8,-11.1,7.));
#14618=CARTESIAN_POINT('',(-2.025,-11.,7.));
#14619=CARTESIAN_POINT('Origin',(-1.8,-11.,7.));
#14620=CARTESIAN_POINT('',(-2.025,-10.4,7.));
#14621=CARTESIAN_POINT('',(-2.025,-11.1,7.));
#14622=CARTESIAN_POINT('Origin',(-1.8,-10.4,7.));
#14623=CARTESIAN_POINT('Origin',(1.10218211923262E-16,-11.1,8.8));
#14624=CARTESIAN_POINT('',(-0.225,-11.,8.8));
#14625=CARTESIAN_POINT('Origin',(1.10218211923262E-16,-11.,8.8));
#14626=CARTESIAN_POINT('',(-0.225,-10.4,8.8));
#14627=CARTESIAN_POINT('',(-0.225,-11.1,8.8));
#14628=CARTESIAN_POINT('Origin',(1.10218211923262E-16,-10.4,8.8));
#14629=CARTESIAN_POINT('Origin',(1.8,-11.1,7.));
#14630=CARTESIAN_POINT('',(1.575,-11.,7.));
#14631=CARTESIAN_POINT('Origin',(1.8,-11.,7.));
#14632=CARTESIAN_POINT('',(1.575,-10.4,7.));
#14633=CARTESIAN_POINT('',(1.575,-11.1,7.));
#14634=CARTESIAN_POINT('Origin',(1.8,-10.4,7.));
#14635=CARTESIAN_POINT('Origin',(-3.30654635769785E-16,-11.1,5.2));
#14636=CARTESIAN_POINT('',(-0.225,-11.,5.2));
#14637=CARTESIAN_POINT('Origin',(-3.30654635769785E-16,-11.,5.2));
#14638=CARTESIAN_POINT('',(-0.225,-10.4,5.2));
#14639=CARTESIAN_POINT('',(-0.225,-11.1,5.2));
#14640=CARTESIAN_POINT('Origin',(-3.30654635769785E-16,-10.4,5.2));
#14641=CARTESIAN_POINT('Origin',(0.,-10.4,7.));
#14642=CARTESIAN_POINT('',(-2.3,-10.4,7.));
#14643=CARTESIAN_POINT('Origin',(0.,-10.4,7.));
#14644=CARTESIAN_POINT('',(-1.5,-10.4,7.));
#14645=CARTESIAN_POINT('Origin',(0.,-10.4,7.));
#14646=CARTESIAN_POINT('Origin',(0.,-11.,7.));
#14647=CARTESIAN_POINT('',(-2.3,-11.,7.));
#14648=CARTESIAN_POINT('',(-2.3,-11.,7.));
#14649=CARTESIAN_POINT('Origin',(0.,-11.,7.));
#14650=CARTESIAN_POINT('Origin',(0.,-11.,7.));
#14651=CARTESIAN_POINT('',(-0.6,-9.2,7.));
#14652=CARTESIAN_POINT('Origin',(0.,-9.2,7.));
#14653=CARTESIAN_POINT('',(-0.6,-11.,7.));
#14654=CARTESIAN_POINT('',(-0.6,-11.,7.));
#14655=CARTESIAN_POINT('Origin',(0.,-11.,7.));
#14656=CARTESIAN_POINT('Origin',(0.,-11.,7.));
#14657=CARTESIAN_POINT('',(-1.5,-9.2,7.));
#14658=CARTESIAN_POINT('Origin',(0.,-9.2,7.));
#14659=CARTESIAN_POINT('',(-1.5,-11.,7.));
#14660=CARTESIAN_POINT('Origin',(0.,-9.2,7.));
#14661=CARTESIAN_POINT('Origin',(0.,-11.,7.));
#14662=CARTESIAN_POINT('',(0.,0.,0.));
#14663=CARTESIAN_POINT('Origin',(0.0721687836487032,0.,-0.125));
#14664=CARTESIAN_POINT('',(0.0721687836487032,0.,-0.125));
#14665=CARTESIAN_POINT('',(0.144337567297406,0.,0.));
#14666=CARTESIAN_POINT('',(0.117710979560879,0.,-0.0461186027918559));
#14667=CARTESIAN_POINT('',(0.0721687836487032,-0.25,-0.125));
#14668=CARTESIAN_POINT('',(0.0721687836487032,0.,-0.125));
#14669=CARTESIAN_POINT('',(0.144337567297406,-0.25,0.));
#14670=CARTESIAN_POINT('',(0.144337567297406,-0.25,0.));
#14671=CARTESIAN_POINT('',(0.144337567297406,0.,0.));
#14672=CARTESIAN_POINT('Origin',(-0.0721687836487032,0.,-0.125));
#14673=CARTESIAN_POINT('',(-0.0721687836487032,0.,-0.125));
#14674=CARTESIAN_POINT('',(0.0739156081756484,0.,-0.125));
#14675=CARTESIAN_POINT('',(-0.0721687836487032,-0.25,-0.125));
#14676=CARTESIAN_POINT('',(-0.0721687836487032,0.,-0.125));
#14677=CARTESIAN_POINT('',(0.0721687836487032,-0.25,-0.125));
#14678=CARTESIAN_POINT('Origin',(-0.144337567297406,0.,-4.16333634234434E-17));
#14679=CARTESIAN_POINT('',(-0.144337567297406,0.,-1.76762539787485E-17));
#14680=CARTESIAN_POINT('',(-0.0987953713852306,0.,-0.0788813972081442));
#14681=CARTESIAN_POINT('',(-0.144337567297406,-0.25,-2.77555756156289E-17));
#14682=CARTESIAN_POINT('',(-0.144337567297406,0.,-1.76762539787485E-17));
#14683=CARTESIAN_POINT('',(-0.0721687836487032,-0.25,-0.125));
#14684=CARTESIAN_POINT('Origin',(-0.0721687836487033,0.,0.125));
#14685=CARTESIAN_POINT('',(-0.0721687836487033,0.,0.125));
#14686=CARTESIAN_POINT('',(-0.0627109795608791,0.,0.141381397208144));
#14687=CARTESIAN_POINT('',(-0.0721687836487033,-0.25,0.125));
#14688=CARTESIAN_POINT('',(-0.0721687836487033,0.,0.125));
#14689=CARTESIAN_POINT('',(-0.144337567297406,-0.25,-1.76762539787485E-17));
#14690=CARTESIAN_POINT('Origin',(0.0721687836487032,0.,0.125));
#14691=CARTESIAN_POINT('',(0.0721687836487032,0.,0.125));
#14692=CARTESIAN_POINT('',(0.146084391824352,0.,0.125));
#14693=CARTESIAN_POINT('',(0.0721687836487032,-0.25,0.125));
#14694=CARTESIAN_POINT('',(0.0721687836487032,0.,0.125));
#14695=CARTESIAN_POINT('',(-0.0721687836487033,-0.25,0.125));
#14696=CARTESIAN_POINT('Origin',(0.144337567297406,0.,0.));
#14697=CARTESIAN_POINT('',(0.153795371385231,0.,-0.0163813972081441));
#14698=CARTESIAN_POINT('',(0.0721687836487032,-0.25,0.125));
#14699=CARTESIAN_POINT('Origin',(0.,-0.25,0.));
#14700=CARTESIAN_POINT('Origin',(0.22,0.,0.));
#14701=CARTESIAN_POINT('',(-0.22,-8.67361737988404E-18,-2.69422295812418E-17));
#14702=CARTESIAN_POINT('Origin',(0.,0.,0.));
#14703=CARTESIAN_POINT('Origin',(0.,-0.015,0.));
#14704=CARTESIAN_POINT('',(-0.24505,-0.02505,-3.00099698131059E-17));
#14705=CARTESIAN_POINT('Origin',(0.,-0.02505,0.));
#14706=CARTESIAN_POINT('',(-0.235,-0.015,-2.87791997799628E-17));
#14707=CARTESIAN_POINT('Origin',(0.,-0.3775,0.));
#14708=CARTESIAN_POINT('',(-0.24505,-0.72995,3.00099698131059E-17));
#14709=CARTESIAN_POINT('Origin',(0.,-0.72995,0.));
#14710=CARTESIAN_POINT('',(-0.24505,-0.3775,-3.00099698131059E-17));
#14711=CARTESIAN_POINT('Origin',(0.,-0.7625,0.));
#14712=CARTESIAN_POINT('',(-0.175,-0.8,-2.14313189850787E-17));
#14713=CARTESIAN_POINT('Origin',(0.,-0.8,0.));
#14714=CARTESIAN_POINT('',(-0.2125,-0.7625,-2.60237444818813E-17));
#14715=CARTESIAN_POINT('Origin',(0.,-0.8,0.));
#14716=CARTESIAN_POINT('',(0.,0.,0.));
#14717=CARTESIAN_POINT('',(0.,0.,0.));
#14718=CARTESIAN_POINT('',(0.,0.,0.));
#14719=CARTESIAN_POINT('',(0.,0.,0.));
#14720=CARTESIAN_POINT('',(0.,0.,0.));
#14721=CARTESIAN_POINT('',(0.,0.,0.));
#14722=CARTESIAN_POINT('',(0.,0.,0.));
#14723=CARTESIAN_POINT('',(0.,0.,0.));
#14724=CARTESIAN_POINT('',(0.,0.,0.));
#14725=CARTESIAN_POINT('',(0.,0.,0.));
#14726=CARTESIAN_POINT('',(0.,-8.6,8.4));
#14727=CARTESIAN_POINT('',(0.,8.6,8.4));
#14728=CARTESIAN_POINT('',(0.,-1.1,8.8));
#14729=CARTESIAN_POINT('',(0.,1.1,8.8));
#14730=CARTESIAN_POINT('',(0.,-9.8,8.4));
#14731=CARTESIAN_POINT('',(0.,0.,0.));
#14732=CARTESIAN_POINT('',(0.,0.,0.));
#14733=UNCERTAINTY_MEASURE_WITH_UNIT(LENGTH_MEASURE(0.001),#14823,
'DISTANCE_ACCURACY_VALUE',
'Maximum model space distance between geometric entities at asserted c
onnectivities');
#14734=UNCERTAINTY_MEASURE_WITH_UNIT(LENGTH_MEASURE(0.001),#14823,
'DISTANCE_ACCURACY_VALUE',
'Maximum model space distance between geometric entities at asserted c
onnectivities');
#14735=UNCERTAINTY_MEASURE_WITH_UNIT(LENGTH_MEASURE(0.001),#14823,
'DISTANCE_ACCURACY_VALUE',
'Maximum model space distance between geometric entities at asserted c
onnectivities');
#14736=UNCERTAINTY_MEASURE_WITH_UNIT(LENGTH_MEASURE(0.001),#14823,
'DISTANCE_ACCURACY_VALUE',
'Maximum model space distance between geometric entities at asserted c
onnectivities');
#14737=UNCERTAINTY_MEASURE_WITH_UNIT(LENGTH_MEASURE(0.001),#14823,
'DISTANCE_ACCURACY_VALUE',
'Maximum model space distance between geometric entities at asserted c
onnectivities');
#14738=UNCERTAINTY_MEASURE_WITH_UNIT(LENGTH_MEASURE(0.001),#14823,
'DISTANCE_ACCURACY_VALUE',
'Maximum model space distance between geometric entities at asserted c
onnectivities');
#14739=UNCERTAINTY_MEASURE_WITH_UNIT(LENGTH_MEASURE(0.001),#14823,
'DISTANCE_ACCURACY_VALUE',
'Maximum model space distance between geometric entities at asserted c
onnectivities');
#14740=UNCERTAINTY_MEASURE_WITH_UNIT(LENGTH_MEASURE(0.001),#14823,
'DISTANCE_ACCURACY_VALUE',
'Maximum model space distance between geometric entities at asserted c
onnectivities');
#14741=UNCERTAINTY_MEASURE_WITH_UNIT(LENGTH_MEASURE(0.001),#14823,
'DISTANCE_ACCURACY_VALUE',
'Maximum model space distance between geometric entities at asserted c
onnectivities');
#14742=UNCERTAINTY_MEASURE_WITH_UNIT(LENGTH_MEASURE(0.001),#14823,
'DISTANCE_ACCURACY_VALUE',
'Maximum model space distance between geometric entities at asserted c
onnectivities');
#14743=UNCERTAINTY_MEASURE_WITH_UNIT(LENGTH_MEASURE(0.001),#14823,
'DISTANCE_ACCURACY_VALUE',
'Maximum model space distance between geometric entities at asserted c
onnectivities');
#14744=UNCERTAINTY_MEASURE_WITH_UNIT(LENGTH_MEASURE(0.001),#14823,
'DISTANCE_ACCURACY_VALUE',
'Maximum model space distance between geometric entities at asserted c
onnectivities');
#14745=UNCERTAINTY_MEASURE_WITH_UNIT(LENGTH_MEASURE(0.001),#14823,
'DISTANCE_ACCURACY_VALUE',
'Maximum model space distance between geometric entities at asserted c
onnectivities');
#14746=UNCERTAINTY_MEASURE_WITH_UNIT(LENGTH_MEASURE(0.001),#14823,
'DISTANCE_ACCURACY_VALUE',
'Maximum model space distance between geometric entities at asserted c
onnectivities');
#14747=UNCERTAINTY_MEASURE_WITH_UNIT(LENGTH_MEASURE(0.001),#14823,
'DISTANCE_ACCURACY_VALUE',
'Maximum model space distance between geometric entities at asserted c
onnectivities');
#14748=UNCERTAINTY_MEASURE_WITH_UNIT(LENGTH_MEASURE(0.001),#14823,
'DISTANCE_ACCURACY_VALUE',
'Maximum model space distance between geometric entities at asserted c
onnectivities');
#14749=UNCERTAINTY_MEASURE_WITH_UNIT(LENGTH_MEASURE(0.001),#14823,
'DISTANCE_ACCURACY_VALUE',
'Maximum model space distance between geometric entities at asserted c
onnectivities');
#14750=UNCERTAINTY_MEASURE_WITH_UNIT(LENGTH_MEASURE(0.001),#14823,
'DISTANCE_ACCURACY_VALUE',
'Maximum model space distance between geometric entities at asserted c
onnectivities');
#14751=UNCERTAINTY_MEASURE_WITH_UNIT(LENGTH_MEASURE(0.001),#14823,
'DISTANCE_ACCURACY_VALUE',
'Maximum model space distance between geometric entities at asserted c
onnectivities');
#14752=UNCERTAINTY_MEASURE_WITH_UNIT(LENGTH_MEASURE(0.001),#14823,
'DISTANCE_ACCURACY_VALUE',
'Maximum model space distance between geometric entities at asserted c
onnectivities');
#14753=UNCERTAINTY_MEASURE_WITH_UNIT(LENGTH_MEASURE(0.001),#14823,
'DISTANCE_ACCURACY_VALUE',
'Maximum model space distance between geometric entities at asserted c
onnectivities');
#14754=UNCERTAINTY_MEASURE_WITH_UNIT(LENGTH_MEASURE(0.001),#14823,
'DISTANCE_ACCURACY_VALUE',
'Maximum model space distance between geometric entities at asserted c
onnectivities');
#14755=UNCERTAINTY_MEASURE_WITH_UNIT(LENGTH_MEASURE(0.001),#14823,
'DISTANCE_ACCURACY_VALUE',
'Maximum model space distance between geometric entities at asserted c
onnectivities');
#14756=UNCERTAINTY_MEASURE_WITH_UNIT(LENGTH_MEASURE(0.001),#14823,
'DISTANCE_ACCURACY_VALUE',
'Maximum model space distance between geometric entities at asserted c
onnectivities');
#14757=UNCERTAINTY_MEASURE_WITH_UNIT(LENGTH_MEASURE(0.001),#14823,
'DISTANCE_ACCURACY_VALUE',
'Maximum model space distance between geometric entities at asserted c
onnectivities');
#14758=UNCERTAINTY_MEASURE_WITH_UNIT(LENGTH_MEASURE(0.001),#14823,
'DISTANCE_ACCURACY_VALUE',
'Maximum model space distance between geometric entities at asserted c
onnectivities');
#14759=UNCERTAINTY_MEASURE_WITH_UNIT(LENGTH_MEASURE(0.001),#14823,
'DISTANCE_ACCURACY_VALUE',
'Maximum model space distance between geometric entities at asserted c
onnectivities');
#14760=UNCERTAINTY_MEASURE_WITH_UNIT(LENGTH_MEASURE(0.001),#14823,
'DISTANCE_ACCURACY_VALUE',
'Maximum model space distance between geometric entities at asserted c
onnectivities');
#14761=UNCERTAINTY_MEASURE_WITH_UNIT(LENGTH_MEASURE(0.001),#14823,
'DISTANCE_ACCURACY_VALUE',
'Maximum model space distance between geometric entities at asserted c
onnectivities');
#14762=UNCERTAINTY_MEASURE_WITH_UNIT(LENGTH_MEASURE(0.001),#14823,
'DISTANCE_ACCURACY_VALUE',
'Maximum model space distance between geometric entities at asserted c
onnectivities');
#14763=UNCERTAINTY_MEASURE_WITH_UNIT(LENGTH_MEASURE(0.001),#14823,
'DISTANCE_ACCURACY_VALUE',
'Maximum model space distance between geometric entities at asserted c
onnectivities');
#14764=UNCERTAINTY_MEASURE_WITH_UNIT(LENGTH_MEASURE(0.001),#14823,
'DISTANCE_ACCURACY_VALUE',
'Maximum model space distance between geometric entities at asserted c
onnectivities');
#14765=UNCERTAINTY_MEASURE_WITH_UNIT(LENGTH_MEASURE(0.001),#14823,
'DISTANCE_ACCURACY_VALUE',
'Maximum model space distance between geometric entities at asserted c
onnectivities');
#14766=UNCERTAINTY_MEASURE_WITH_UNIT(LENGTH_MEASURE(0.001),#14823,
'DISTANCE_ACCURACY_VALUE',
'Maximum model space distance between geometric entities at asserted c
onnectivities');
#14767=UNCERTAINTY_MEASURE_WITH_UNIT(LENGTH_MEASURE(0.001),#14823,
'DISTANCE_ACCURACY_VALUE',
'Maximum model space distance between geometric entities at asserted c
onnectivities');
#14768=UNCERTAINTY_MEASURE_WITH_UNIT(LENGTH_MEASURE(0.001),#14823,
'DISTANCE_ACCURACY_VALUE',
'Maximum model space distance between geometric entities at asserted c
onnectivities');
#14769=UNCERTAINTY_MEASURE_WITH_UNIT(LENGTH_MEASURE(0.001),#14823,
'DISTANCE_ACCURACY_VALUE',
'Maximum model space distance between geometric entities at asserted c
onnectivities');
#14770=UNCERTAINTY_MEASURE_WITH_UNIT(LENGTH_MEASURE(0.001),#14823,
'DISTANCE_ACCURACY_VALUE',
'Maximum model space distance between geometric entities at asserted c
onnectivities');
#14771=UNCERTAINTY_MEASURE_WITH_UNIT(LENGTH_MEASURE(0.001),#14823,
'DISTANCE_ACCURACY_VALUE',
'Maximum model space distance between geometric entities at asserted c
onnectivities');
#14772=UNCERTAINTY_MEASURE_WITH_UNIT(LENGTH_MEASURE(0.001),#14823,
'DISTANCE_ACCURACY_VALUE',
'Maximum model space distance between geometric entities at asserted c
onnectivities');
#14773=UNCERTAINTY_MEASURE_WITH_UNIT(LENGTH_MEASURE(0.001),#14823,
'DISTANCE_ACCURACY_VALUE',
'Maximum model space distance between geometric entities at asserted c
onnectivities');
#14774=UNCERTAINTY_MEASURE_WITH_UNIT(LENGTH_MEASURE(0.001),#14823,
'DISTANCE_ACCURACY_VALUE',
'Maximum model space distance between geometric entities at asserted c
onnectivities');
#14775=UNCERTAINTY_MEASURE_WITH_UNIT(LENGTH_MEASURE(0.001),#14823,
'DISTANCE_ACCURACY_VALUE',
'Maximum model space distance between geometric entities at asserted c
onnectivities');
#14776=UNCERTAINTY_MEASURE_WITH_UNIT(LENGTH_MEASURE(0.001),#14823,
'DISTANCE_ACCURACY_VALUE',
'Maximum model space distance between geometric entities at asserted c
onnectivities');
#14777=UNCERTAINTY_MEASURE_WITH_UNIT(LENGTH_MEASURE(0.001),#14823,
'DISTANCE_ACCURACY_VALUE',
'Maximum model space distance between geometric entities at asserted c
onnectivities');
#14778=(
GEOMETRIC_REPRESENTATION_CONTEXT(3)
GLOBAL_UNCERTAINTY_ASSIGNED_CONTEXT((#14733))
GLOBAL_UNIT_ASSIGNED_CONTEXT((#14823,#14825,#14826))
REPRESENTATION_CONTEXT('','3D')
);
#14779=(
GEOMETRIC_REPRESENTATION_CONTEXT(3)
GLOBAL_UNCERTAINTY_ASSIGNED_CONTEXT((#14734))
GLOBAL_UNIT_ASSIGNED_CONTEXT((#14823,#14825,#14826))
REPRESENTATION_CONTEXT('','3D')
);
#14780=(
GEOMETRIC_REPRESENTATION_CONTEXT(3)
GLOBAL_UNCERTAINTY_ASSIGNED_CONTEXT((#14735))
GLOBAL_UNIT_ASSIGNED_CONTEXT((#14823,#14825,#14826))
REPRESENTATION_CONTEXT('','3D')
);
#14781=(
GEOMETRIC_REPRESENTATION_CONTEXT(3)
GLOBAL_UNCERTAINTY_ASSIGNED_CONTEXT((#14736))
GLOBAL_UNIT_ASSIGNED_CONTEXT((#14823,#14825,#14826))
REPRESENTATION_CONTEXT('','3D')
);
#14782=(
GEOMETRIC_REPRESENTATION_CONTEXT(3)
GLOBAL_UNCERTAINTY_ASSIGNED_CONTEXT((#14737))
GLOBAL_UNIT_ASSIGNED_CONTEXT((#14823,#14825,#14826))
REPRESENTATION_CONTEXT('','3D')
);
#14783=(
GEOMETRIC_REPRESENTATION_CONTEXT(3)
GLOBAL_UNCERTAINTY_ASSIGNED_CONTEXT((#14738))
GLOBAL_UNIT_ASSIGNED_CONTEXT((#14823,#14825,#14826))
REPRESENTATION_CONTEXT('','3D')
);
#14784=(
GEOMETRIC_REPRESENTATION_CONTEXT(3)
GLOBAL_UNCERTAINTY_ASSIGNED_CONTEXT((#14739))
GLOBAL_UNIT_ASSIGNED_CONTEXT((#14823,#14825,#14826))
REPRESENTATION_CONTEXT('','3D')
);
#14785=(
GEOMETRIC_REPRESENTATION_CONTEXT(3)
GLOBAL_UNCERTAINTY_ASSIGNED_CONTEXT((#14740))
GLOBAL_UNIT_ASSIGNED_CONTEXT((#14823,#14825,#14826))
REPRESENTATION_CONTEXT('','3D')
);
#14786=(
GEOMETRIC_REPRESENTATION_CONTEXT(3)
GLOBAL_UNCERTAINTY_ASSIGNED_CONTEXT((#14741))
GLOBAL_UNIT_ASSIGNED_CONTEXT((#14823,#14825,#14826))
REPRESENTATION_CONTEXT('','3D')
);
#14787=(
GEOMETRIC_REPRESENTATION_CONTEXT(3)
GLOBAL_UNCERTAINTY_ASSIGNED_CONTEXT((#14742))
GLOBAL_UNIT_ASSIGNED_CONTEXT((#14823,#14825,#14826))
REPRESENTATION_CONTEXT('','3D')
);
#14788=(
GEOMETRIC_REPRESENTATION_CONTEXT(3)
GLOBAL_UNCERTAINTY_ASSIGNED_CONTEXT((#14743))
GLOBAL_UNIT_ASSIGNED_CONTEXT((#14823,#14825,#14826))
REPRESENTATION_CONTEXT('','3D')
);
#14789=(
GEOMETRIC_REPRESENTATION_CONTEXT(3)
GLOBAL_UNCERTAINTY_ASSIGNED_CONTEXT((#14744))
GLOBAL_UNIT_ASSIGNED_CONTEXT((#14823,#14825,#14826))
REPRESENTATION_CONTEXT('','3D')
);
#14790=(
GEOMETRIC_REPRESENTATION_CONTEXT(3)
GLOBAL_UNCERTAINTY_ASSIGNED_CONTEXT((#14745))
GLOBAL_UNIT_ASSIGNED_CONTEXT((#14823,#14825,#14826))
REPRESENTATION_CONTEXT('','3D')
);
#14791=(
GEOMETRIC_REPRESENTATION_CONTEXT(3)
GLOBAL_UNCERTAINTY_ASSIGNED_CONTEXT((#14746))
GLOBAL_UNIT_ASSIGNED_CONTEXT((#14823,#14825,#14826))
REPRESENTATION_CONTEXT('','3D')
);
#14792=(
GEOMETRIC_REPRESENTATION_CONTEXT(3)
GLOBAL_UNCERTAINTY_ASSIGNED_CONTEXT((#14747))
GLOBAL_UNIT_ASSIGNED_CONTEXT((#14823,#14825,#14826))
REPRESENTATION_CONTEXT('','3D')
);
#14793=(
GEOMETRIC_REPRESENTATION_CONTEXT(3)
GLOBAL_UNCERTAINTY_ASSIGNED_CONTEXT((#14748))
GLOBAL_UNIT_ASSIGNED_CONTEXT((#14823,#14825,#14826))
REPRESENTATION_CONTEXT('','3D')
);
#14794=(
GEOMETRIC_REPRESENTATION_CONTEXT(3)
GLOBAL_UNCERTAINTY_ASSIGNED_CONTEXT((#14749))
GLOBAL_UNIT_ASSIGNED_CONTEXT((#14823,#14825,#14826))
REPRESENTATION_CONTEXT('','3D')
);
#14795=(
GEOMETRIC_REPRESENTATION_CONTEXT(3)
GLOBAL_UNCERTAINTY_ASSIGNED_CONTEXT((#14750))
GLOBAL_UNIT_ASSIGNED_CONTEXT((#14823,#14825,#14826))
REPRESENTATION_CONTEXT('','3D')
);
#14796=(
GEOMETRIC_REPRESENTATION_CONTEXT(3)
GLOBAL_UNCERTAINTY_ASSIGNED_CONTEXT((#14751))
GLOBAL_UNIT_ASSIGNED_CONTEXT((#14823,#14825,#14826))
REPRESENTATION_CONTEXT('','3D')
);
#14797=(
GEOMETRIC_REPRESENTATION_CONTEXT(3)
GLOBAL_UNCERTAINTY_ASSIGNED_CONTEXT((#14752))
GLOBAL_UNIT_ASSIGNED_CONTEXT((#14823,#14825,#14826))
REPRESENTATION_CONTEXT('','3D')
);
#14798=(
GEOMETRIC_REPRESENTATION_CONTEXT(3)
GLOBAL_UNCERTAINTY_ASSIGNED_CONTEXT((#14753))
GLOBAL_UNIT_ASSIGNED_CONTEXT((#14823,#14825,#14826))
REPRESENTATION_CONTEXT('','3D')
);
#14799=(
GEOMETRIC_REPRESENTATION_CONTEXT(3)
GLOBAL_UNCERTAINTY_ASSIGNED_CONTEXT((#14754))
GLOBAL_UNIT_ASSIGNED_CONTEXT((#14823,#14825,#14826))
REPRESENTATION_CONTEXT('','3D')
);
#14800=(
GEOMETRIC_REPRESENTATION_CONTEXT(3)
GLOBAL_UNCERTAINTY_ASSIGNED_CONTEXT((#14755))
GLOBAL_UNIT_ASSIGNED_CONTEXT((#14823,#14825,#14826))
REPRESENTATION_CONTEXT('','3D')
);
#14801=(
GEOMETRIC_REPRESENTATION_CONTEXT(3)
GLOBAL_UNCERTAINTY_ASSIGNED_CONTEXT((#14756))
GLOBAL_UNIT_ASSIGNED_CONTEXT((#14823,#14825,#14826))
REPRESENTATION_CONTEXT('','3D')
);
#14802=(
GEOMETRIC_REPRESENTATION_CONTEXT(3)
GLOBAL_UNCERTAINTY_ASSIGNED_CONTEXT((#14757))
GLOBAL_UNIT_ASSIGNED_CONTEXT((#14823,#14825,#14826))
REPRESENTATION_CONTEXT('','3D')
);
#14803=(
GEOMETRIC_REPRESENTATION_CONTEXT(3)
GLOBAL_UNCERTAINTY_ASSIGNED_CONTEXT((#14758))
GLOBAL_UNIT_ASSIGNED_CONTEXT((#14823,#14825,#14826))
REPRESENTATION_CONTEXT('','3D')
);
#14804=(
GEOMETRIC_REPRESENTATION_CONTEXT(3)
GLOBAL_UNCERTAINTY_ASSIGNED_CONTEXT((#14759))
GLOBAL_UNIT_ASSIGNED_CONTEXT((#14823,#14825,#14826))
REPRESENTATION_CONTEXT('','3D')
);
#14805=(
GEOMETRIC_REPRESENTATION_CONTEXT(3)
GLOBAL_UNCERTAINTY_ASSIGNED_CONTEXT((#14760))
GLOBAL_UNIT_ASSIGNED_CONTEXT((#14823,#14825,#14826))
REPRESENTATION_CONTEXT('','3D')
);
#14806=(
GEOMETRIC_REPRESENTATION_CONTEXT(3)
GLOBAL_UNCERTAINTY_ASSIGNED_CONTEXT((#14761))
GLOBAL_UNIT_ASSIGNED_CONTEXT((#14823,#14825,#14826))
REPRESENTATION_CONTEXT('','3D')
);
#14807=(
GEOMETRIC_REPRESENTATION_CONTEXT(3)
GLOBAL_UNCERTAINTY_ASSIGNED_CONTEXT((#14762))
GLOBAL_UNIT_ASSIGNED_CONTEXT((#14823,#14825,#14826))
REPRESENTATION_CONTEXT('','3D')
);
#14808=(
GEOMETRIC_REPRESENTATION_CONTEXT(3)
GLOBAL_UNCERTAINTY_ASSIGNED_CONTEXT((#14763))
GLOBAL_UNIT_ASSIGNED_CONTEXT((#14823,#14825,#14826))
REPRESENTATION_CONTEXT('','3D')
);
#14809=(
GEOMETRIC_REPRESENTATION_CONTEXT(3)
GLOBAL_UNCERTAINTY_ASSIGNED_CONTEXT((#14764))
GLOBAL_UNIT_ASSIGNED_CONTEXT((#14823,#14825,#14826))
REPRESENTATION_CONTEXT('','3D')
);
#14810=(
GEOMETRIC_REPRESENTATION_CONTEXT(3)
GLOBAL_UNCERTAINTY_ASSIGNED_CONTEXT((#14765))
GLOBAL_UNIT_ASSIGNED_CONTEXT((#14823,#14825,#14826))
REPRESENTATION_CONTEXT('','3D')
);
#14811=(
GEOMETRIC_REPRESENTATION_CONTEXT(3)
GLOBAL_UNCERTAINTY_ASSIGNED_CONTEXT((#14766))
GLOBAL_UNIT_ASSIGNED_CONTEXT((#14823,#14825,#14826))
REPRESENTATION_CONTEXT('','3D')
);
#14812=(
GEOMETRIC_REPRESENTATION_CONTEXT(3)
GLOBAL_UNCERTAINTY_ASSIGNED_CONTEXT((#14767))
GLOBAL_UNIT_ASSIGNED_CONTEXT((#14823,#14825,#14826))
REPRESENTATION_CONTEXT('','3D')
);
#14813=(
GEOMETRIC_REPRESENTATION_CONTEXT(3)
GLOBAL_UNCERTAINTY_ASSIGNED_CONTEXT((#14768))
GLOBAL_UNIT_ASSIGNED_CONTEXT((#14823,#14825,#14826))
REPRESENTATION_CONTEXT('','3D')
);
#14814=(
GEOMETRIC_REPRESENTATION_CONTEXT(3)
GLOBAL_UNCERTAINTY_ASSIGNED_CONTEXT((#14769))
GLOBAL_UNIT_ASSIGNED_CONTEXT((#14823,#14825,#14826))
REPRESENTATION_CONTEXT('','3D')
);
#14815=(
GEOMETRIC_REPRESENTATION_CONTEXT(3)
GLOBAL_UNCERTAINTY_ASSIGNED_CONTEXT((#14770))
GLOBAL_UNIT_ASSIGNED_CONTEXT((#14823,#14825,#14826))
REPRESENTATION_CONTEXT('','3D')
);
#14816=(
GEOMETRIC_REPRESENTATION_CONTEXT(3)
GLOBAL_UNCERTAINTY_ASSIGNED_CONTEXT((#14771))
GLOBAL_UNIT_ASSIGNED_CONTEXT((#14823,#14825,#14826))
REPRESENTATION_CONTEXT('','3D')
);
#14817=(
GEOMETRIC_REPRESENTATION_CONTEXT(3)
GLOBAL_UNCERTAINTY_ASSIGNED_CONTEXT((#14772))
GLOBAL_UNIT_ASSIGNED_CONTEXT((#14823,#14825,#14826))
REPRESENTATION_CONTEXT('','3D')
);
#14818=(
GEOMETRIC_REPRESENTATION_CONTEXT(3)
GLOBAL_UNCERTAINTY_ASSIGNED_CONTEXT((#14773))
GLOBAL_UNIT_ASSIGNED_CONTEXT((#14823,#14825,#14826))
REPRESENTATION_CONTEXT('','3D')
);
#14819=(
GEOMETRIC_REPRESENTATION_CONTEXT(3)
GLOBAL_UNCERTAINTY_ASSIGNED_CONTEXT((#14774))
GLOBAL_UNIT_ASSIGNED_CONTEXT((#14823,#14825,#14826))
REPRESENTATION_CONTEXT('','3D')
);
#14820=(
GEOMETRIC_REPRESENTATION_CONTEXT(3)
GLOBAL_UNCERTAINTY_ASSIGNED_CONTEXT((#14775))
GLOBAL_UNIT_ASSIGNED_CONTEXT((#14823,#14825,#14826))
REPRESENTATION_CONTEXT('','3D')
);
#14821=(
GEOMETRIC_REPRESENTATION_CONTEXT(3)
GLOBAL_UNCERTAINTY_ASSIGNED_CONTEXT((#14776))
GLOBAL_UNIT_ASSIGNED_CONTEXT((#14823,#14825,#14826))
REPRESENTATION_CONTEXT('','3D')
);
#14822=(
GEOMETRIC_REPRESENTATION_CONTEXT(3)
GLOBAL_UNCERTAINTY_ASSIGNED_CONTEXT((#14777))
GLOBAL_UNIT_ASSIGNED_CONTEXT((#14823,#14825,#14826))
REPRESENTATION_CONTEXT('','3D')
);
#14823=(
LENGTH_UNIT()
NAMED_UNIT(*)
SI_UNIT(.CENTI.,.METRE.)
);
#14824=(
LENGTH_UNIT()
NAMED_UNIT(*)
SI_UNIT($,.METRE.)
);
#14825=(
NAMED_UNIT(*)
PLANE_ANGLE_UNIT()
SI_UNIT($,.RADIAN.)
);
#14826=(
NAMED_UNIT(*)
SI_UNIT($,.STERADIAN.)
SOLID_ANGLE_UNIT()
);
#14827=SHAPE_DEFINITION_REPRESENTATION(#14871,#14998);
#14828=SHAPE_DEFINITION_REPRESENTATION(#14872,#14999);
#14829=SHAPE_DEFINITION_REPRESENTATION(#14873,#15000);
#14830=SHAPE_DEFINITION_REPRESENTATION(#14874,#15001);
#14831=SHAPE_DEFINITION_REPRESENTATION(#14875,#15002);
#14832=SHAPE_DEFINITION_REPRESENTATION(#14876,#15003);
#14833=SHAPE_DEFINITION_REPRESENTATION(#14877,#15004);
#14834=SHAPE_DEFINITION_REPRESENTATION(#14878,#15005);
#14835=SHAPE_DEFINITION_REPRESENTATION(#14879,#15006);
#14836=SHAPE_DEFINITION_REPRESENTATION(#14880,#15007);
#14837=SHAPE_DEFINITION_REPRESENTATION(#14881,#15008);
#14838=SHAPE_DEFINITION_REPRESENTATION(#14882,#15009);
#14839=SHAPE_DEFINITION_REPRESENTATION(#14883,#15010);
#14840=SHAPE_DEFINITION_REPRESENTATION(#14884,#15011);
#14841=SHAPE_DEFINITION_REPRESENTATION(#14885,#15012);
#14842=SHAPE_DEFINITION_REPRESENTATION(#14886,#15013);
#14843=SHAPE_DEFINITION_REPRESENTATION(#14887,#15014);
#14844=SHAPE_DEFINITION_REPRESENTATION(#14888,#15015);
#14845=SHAPE_DEFINITION_REPRESENTATION(#14889,#15016);
#14846=SHAPE_DEFINITION_REPRESENTATION(#14890,#15017);
#14847=SHAPE_DEFINITION_REPRESENTATION(#14891,#15018);
#14848=SHAPE_DEFINITION_REPRESENTATION(#14892,#15019);
#14849=SHAPE_DEFINITION_REPRESENTATION(#14893,#15020);
#14850=SHAPE_DEFINITION_REPRESENTATION(#14894,#15021);
#14851=SHAPE_DEFINITION_REPRESENTATION(#14900,#15022);
#14852=SHAPE_DEFINITION_REPRESENTATION(#14901,#15023);
#14853=SHAPE_DEFINITION_REPRESENTATION(#14902,#15024);
#14854=SHAPE_DEFINITION_REPRESENTATION(#14903,#15025);
#14855=SHAPE_DEFINITION_REPRESENTATION(#14904,#15026);
#14856=SHAPE_DEFINITION_REPRESENTATION(#14905,#15027);
#14857=SHAPE_DEFINITION_REPRESENTATION(#14911,#15028);
#14858=SHAPE_DEFINITION_REPRESENTATION(#14912,#15029);
#14859=SHAPE_DEFINITION_REPRESENTATION(#14969,#15030);
#14860=SHAPE_DEFINITION_REPRESENTATION(#14970,#15031);
#14861=SHAPE_DEFINITION_REPRESENTATION(#14971,#15032);
#14862=SHAPE_DEFINITION_REPRESENTATION(#14972,#15033);
#14863=SHAPE_DEFINITION_REPRESENTATION(#14973,#15034);
#14864=SHAPE_DEFINITION_REPRESENTATION(#14974,#15035);
#14865=SHAPE_DEFINITION_REPRESENTATION(#14975,#15036);
#14866=SHAPE_DEFINITION_REPRESENTATION(#14976,#15037);
#14867=SHAPE_DEFINITION_REPRESENTATION(#14977,#15038);
#14868=SHAPE_DEFINITION_REPRESENTATION(#14978,#15039);
#14869=SHAPE_DEFINITION_REPRESENTATION(#14979,#15040);
#14870=SHAPE_DEFINITION_REPRESENTATION(#14980,#15041);
#14871=PRODUCT_DEFINITION_SHAPE('',$,#15043);
#14872=PRODUCT_DEFINITION_SHAPE('',$,#15044);
#14873=PRODUCT_DEFINITION_SHAPE('',$,#15045);
#14874=PRODUCT_DEFINITION_SHAPE('',$,#15046);
#14875=PRODUCT_DEFINITION_SHAPE('',$,#15047);
#14876=PRODUCT_DEFINITION_SHAPE('',$,#15048);
#14877=PRODUCT_DEFINITION_SHAPE('',$,#15049);
#14878=PRODUCT_DEFINITION_SHAPE('',$,#15050);
#14879=PRODUCT_DEFINITION_SHAPE('',$,#15051);
#14880=PRODUCT_DEFINITION_SHAPE('',$,#15052);
#14881=PRODUCT_DEFINITION_SHAPE('',$,#15053);
#14882=PRODUCT_DEFINITION_SHAPE('',$,#15054);
#14883=PRODUCT_DEFINITION_SHAPE('',$,#15055);
#14884=PRODUCT_DEFINITION_SHAPE('',$,#15056);
#14885=PRODUCT_DEFINITION_SHAPE('',$,#15057);
#14886=PRODUCT_DEFINITION_SHAPE('',$,#15058);
#14887=PRODUCT_DEFINITION_SHAPE('',$,#15059);
#14888=PRODUCT_DEFINITION_SHAPE('',$,#15060);
#14889=PRODUCT_DEFINITION_SHAPE('',$,#15061);
#14890=PRODUCT_DEFINITION_SHAPE('',$,#15062);
#14891=PRODUCT_DEFINITION_SHAPE('',$,#15063);
#14892=PRODUCT_DEFINITION_SHAPE('',$,#15064);
#14893=PRODUCT_DEFINITION_SHAPE('',$,#15065);
#14894=PRODUCT_DEFINITION_SHAPE('',$,#15066);
#14895=PRODUCT_DEFINITION_SHAPE($,$,#260);
#14896=PRODUCT_DEFINITION_SHAPE($,$,#261);
#14897=PRODUCT_DEFINITION_SHAPE($,$,#262);
#14898=PRODUCT_DEFINITION_SHAPE($,$,#263);
#14899=PRODUCT_DEFINITION_SHAPE($,$,#264);
#14900=PRODUCT_DEFINITION_SHAPE('',$,#15067);
#14901=PRODUCT_DEFINITION_SHAPE('',$,#15068);
#14902=PRODUCT_DEFINITION_SHAPE('',$,#15069);
#14903=PRODUCT_DEFINITION_SHAPE('',$,#15070);
#14904=PRODUCT_DEFINITION_SHAPE('',$,#15071);
#14905=PRODUCT_DEFINITION_SHAPE('',$,#15072);
#14906=PRODUCT_DEFINITION_SHAPE($,$,#265);
#14907=PRODUCT_DEFINITION_SHAPE($,$,#266);
#14908=PRODUCT_DEFINITION_SHAPE($,$,#267);
#14909=PRODUCT_DEFINITION_SHAPE($,$,#268);
#14910=PRODUCT_DEFINITION_SHAPE($,$,#269);
#14911=PRODUCT_DEFINITION_SHAPE('',$,#15073);
#14912=PRODUCT_DEFINITION_SHAPE('',$,#15074);
#14913=PRODUCT_DEFINITION_SHAPE($,$,#270);
#14914=PRODUCT_DEFINITION_SHAPE($,$,#271);
#14915=PRODUCT_DEFINITION_SHAPE($,$,#272);
#14916=PRODUCT_DEFINITION_SHAPE($,$,#273);
#14917=PRODUCT_DEFINITION_SHAPE($,$,#274);
#14918=PRODUCT_DEFINITION_SHAPE($,$,#275);
#14919=PRODUCT_DEFINITION_SHAPE($,$,#276);
#14920=PRODUCT_DEFINITION_SHAPE($,$,#277);
#14921=PRODUCT_DEFINITION_SHAPE($,$,#278);
#14922=PRODUCT_DEFINITION_SHAPE($,$,#279);
#14923=PRODUCT_DEFINITION_SHAPE($,$,#280);
#14924=PRODUCT_DEFINITION_SHAPE($,$,#281);
#14925=PRODUCT_DEFINITION_SHAPE($,$,#282);
#14926=PRODUCT_DEFINITION_SHAPE($,$,#283);
#14927=PRODUCT_DEFINITION_SHAPE($,$,#284);
#14928=PRODUCT_DEFINITION_SHAPE($,$,#285);
#14929=PRODUCT_DEFINITION_SHAPE($,$,#286);
#14930=PRODUCT_DEFINITION_SHAPE($,$,#287);
#14931=PRODUCT_DEFINITION_SHAPE($,$,#288);
#14932=PRODUCT_DEFINITION_SHAPE($,$,#289);
#14933=PRODUCT_DEFINITION_SHAPE($,$,#290);
#14934=PRODUCT_DEFINITION_SHAPE($,$,#291);
#14935=PRODUCT_DEFINITION_SHAPE($,$,#292);
#14936=PRODUCT_DEFINITION_SHAPE($,$,#293);
#14937=PRODUCT_DEFINITION_SHAPE($,$,#294);
#14938=PRODUCT_DEFINITION_SHAPE($,$,#295);
#14939=PRODUCT_DEFINITION_SHAPE($,$,#296);
#14940=PRODUCT_DEFINITION_SHAPE($,$,#297);
#14941=PRODUCT_DEFINITION_SHAPE($,$,#298);
#14942=PRODUCT_DEFINITION_SHAPE($,$,#299);
#14943=PRODUCT_DEFINITION_SHAPE($,$,#300);
#14944=PRODUCT_DEFINITION_SHAPE($,$,#301);
#14945=PRODUCT_DEFINITION_SHAPE($,$,#302);
#14946=PRODUCT_DEFINITION_SHAPE($,$,#303);
#14947=PRODUCT_DEFINITION_SHAPE($,$,#304);
#14948=PRODUCT_DEFINITION_SHAPE($,$,#305);
#14949=PRODUCT_DEFINITION_SHAPE($,$,#306);
#14950=PRODUCT_DEFINITION_SHAPE($,$,#307);
#14951=PRODUCT_DEFINITION_SHAPE($,$,#308);
#14952=PRODUCT_DEFINITION_SHAPE($,$,#309);
#14953=PRODUCT_DEFINITION_SHAPE($,$,#310);
#14954=PRODUCT_DEFINITION_SHAPE($,$,#311);
#14955=PRODUCT_DEFINITION_SHAPE($,$,#312);
#14956=PRODUCT_DEFINITION_SHAPE($,$,#313);
#14957=PRODUCT_DEFINITION_SHAPE($,$,#314);
#14958=PRODUCT_DEFINITION_SHAPE($,$,#315);
#14959=PRODUCT_DEFINITION_SHAPE($,$,#316);
#14960=PRODUCT_DEFINITION_SHAPE($,$,#317);
#14961=PRODUCT_DEFINITION_SHAPE($,$,#318);
#14962=PRODUCT_DEFINITION_SHAPE($,$,#319);
#14963=PRODUCT_DEFINITION_SHAPE($,$,#320);
#14964=PRODUCT_DEFINITION_SHAPE($,$,#321);
#14965=PRODUCT_DEFINITION_SHAPE($,$,#322);
#14966=PRODUCT_DEFINITION_SHAPE($,$,#323);
#14967=PRODUCT_DEFINITION_SHAPE($,$,#324);
#14968=PRODUCT_DEFINITION_SHAPE($,$,#325);
#14969=PRODUCT_DEFINITION_SHAPE('',$,#15075);
#14970=PRODUCT_DEFINITION_SHAPE('',$,#15076);
#14971=PRODUCT_DEFINITION_SHAPE('',$,#15077);
#14972=PRODUCT_DEFINITION_SHAPE('',$,#15078);
#14973=PRODUCT_DEFINITION_SHAPE('',$,#15079);
#14974=PRODUCT_DEFINITION_SHAPE('',$,#15080);
#14975=PRODUCT_DEFINITION_SHAPE('',$,#15081);
#14976=PRODUCT_DEFINITION_SHAPE('',$,#15082);
#14977=PRODUCT_DEFINITION_SHAPE('',$,#15083);
#14978=PRODUCT_DEFINITION_SHAPE('',$,#15084);
#14979=PRODUCT_DEFINITION_SHAPE('',$,#15085);
#14980=PRODUCT_DEFINITION_SHAPE('',$,#15086);
#14981=PRODUCT_DEFINITION_SHAPE($,$,#326);
#14982=PRODUCT_DEFINITION_SHAPE($,$,#327);
#14983=PRODUCT_DEFINITION_SHAPE($,$,#328);
#14984=PRODUCT_DEFINITION_SHAPE($,$,#329);
#14985=PRODUCT_DEFINITION_SHAPE($,$,#330);
#14986=PRODUCT_DEFINITION_SHAPE($,$,#331);
#14987=PRODUCT_DEFINITION_SHAPE($,$,#332);
#14988=PRODUCT_DEFINITION_SHAPE($,$,#333);
#14989=PRODUCT_DEFINITION_SHAPE($,$,#334);
#14990=PRODUCT_DEFINITION_SHAPE($,$,#335);
#14991=PRODUCT_DEFINITION_SHAPE($,$,#336);
#14992=PRODUCT_DEFINITION_SHAPE($,$,#337);
#14993=PRODUCT_DEFINITION_SHAPE($,$,#338);
#14994=PRODUCT_DEFINITION_SHAPE($,$,#339);
#14995=PRODUCT_DEFINITION_SHAPE($,$,#340);
#14996=PRODUCT_DEFINITION_SHAPE($,$,#341);
#14997=PRODUCT_DEFINITION_SHAPE($,$,#342);
#14998=SHAPE_REPRESENTATION('',(#8142,#9164,#9165),#14778);
#14999=SHAPE_REPRESENTATION('',(#8143,#8934,#8935,#8936,#8937,#8938,#8939,
#8940,#8941,#8942,#8943,#8944,#8945,#8946,#8947,#8948,#8949,#8950,#8951,
#8952,#8953,#8954,#8955,#8956,#8957,#8958,#8959,#8960,#8961,#8962,#8963,
#8964,#8965,#8966,#8967,#8968,#8969,#8970,#8971,#8972,#8973,#8974,#8975,
#8976,#8977,#8978,#8979,#8980,#8981,#8982,#8983,#8984,#8985,#8986,#8987,
#8988,#8989),#14779);
#15000=SHAPE_REPRESENTATION('',(#8144),#14780);
#15001=SHAPE_REPRESENTATION('',(#8187),#14781);
#15002=SHAPE_REPRESENTATION('',(#8233),#14782);
#15003=SHAPE_REPRESENTATION('',(#8258),#14783);
#15004=SHAPE_REPRESENTATION('',(#8283),#14784);
#15005=SHAPE_REPRESENTATION('',(#8329),#14785);
#15006=SHAPE_REPRESENTATION('',(#8354),#14786);
#15007=SHAPE_REPRESENTATION('',(#8379),#14787);
#15008=SHAPE_REPRESENTATION('',(#8407),#14788);
#15009=SHAPE_REPRESENTATION('',(#8432),#14789);
#15010=SHAPE_REPRESENTATION('',(#8457),#14790);
#15011=SHAPE_REPRESENTATION('',(#8500),#14791);
#15012=SHAPE_REPRESENTATION('',(#8517),#14792);
#15013=SHAPE_REPRESENTATION('',(#8584),#14793);
#15014=SHAPE_REPRESENTATION('',(#8591),#14794);
#15015=SHAPE_REPRESENTATION('',(#8598),#14795);
#15016=SHAPE_REPRESENTATION('',(#8622,#8745,#8746,#8747,#8748,#8749),#14796);
#15017=SHAPE_REPRESENTATION('',(#8623),#14797);
#15018=SHAPE_REPRESENTATION('',(#8643),#14798);
#15019=SHAPE_REPRESENTATION('',(#8663),#14799);
#15020=SHAPE_REPRESENTATION('',(#8678),#14800);
#15021=SHAPE_REPRESENTATION('',(#8728),#14801);
#15022=SHAPE_REPRESENTATION('',(#8750,#8879,#8880,#8881,#8882,#8883),#14802);
#15023=SHAPE_REPRESENTATION('',(#8751),#14803);
#15024=SHAPE_REPRESENTATION('',(#8771),#14804);
#15025=SHAPE_REPRESENTATION('',(#8791),#14805);
#15026=SHAPE_REPRESENTATION('',(#8808),#14806);
#15027=SHAPE_REPRESENTATION('',(#8862),#14807);
#15028=SHAPE_REPRESENTATION('',(#8884),#14808);
#15029=SHAPE_REPRESENTATION('',(#8910),#14809);
#15030=SHAPE_REPRESENTATION('',(#8990,#9149,#9150,#9151,#9152,#9153,#9154,
#9155,#9156,#9157,#9158,#9159,#9160,#9161,#9162,#9163),#14810);
#15031=SHAPE_REPRESENTATION('',(#8991),#14811);
#15032=SHAPE_REPRESENTATION('',(#9005),#14812);
#15033=SHAPE_REPRESENTATION('',(#9014),#14813);
#15034=SHAPE_REPRESENTATION('',(#9023),#14814);
#15035=SHAPE_REPRESENTATION('',(#9038),#14815);
#15036=SHAPE_REPRESENTATION('',(#9053),#14816);
#15037=SHAPE_REPRESENTATION('',(#9062),#14817);
#15038=SHAPE_REPRESENTATION('',(#9071),#14818);
#15039=SHAPE_REPRESENTATION('',(#9086),#14819);
#15040=SHAPE_REPRESENTATION('',(#9101),#14820);
#15041=SHAPE_REPRESENTATION('',(#9132),#14821);
#15042=PRODUCT_DEFINITION_CONTEXT('part definition',#15176,'design');
#15043=PRODUCT_DEFINITION('PAT-007','PAT-007',
#15087,#15042);
#15044=PRODUCT_DEFINITION('Supports and reaction sensor',
'Supports and reaction sensor',#15088,#15042);
#15045=PRODUCT_DEFINITION('Base','Base',#15089,#15042);
#15046=PRODUCT_DEFINITION('Support housing','Support housing',#15090,#15042);
#15047=PRODUCT_DEFINITION('Support cap','Support cap',#15091,#15042);
#15048=PRODUCT_DEFINITION('Support cap (1)','Support cap (1)',#15092,#15042);
#15049=PRODUCT_DEFINITION('Support housing (1)','Support housing (1)',#15093,
#15042);
#15050=PRODUCT_DEFINITION('Support cap (2)','Support cap (2)',#15094,#15042);
#15051=PRODUCT_DEFINITION('Support cap (3)','Support cap (3)',#15095,#15042);
#15052=PRODUCT_DEFINITION('Reaction housing and arm',
'Reaction housing and arm',#15096,#15042);
#15053=PRODUCT_DEFINITION('Test bearing cap','Test bearing cap',#15097,
#15042);
#15054=PRODUCT_DEFINITION('Test bearing cap (1)','Test bearing cap (1)',#15098,
#15042);
#15055=PRODUCT_DEFINITION('Sensor pedestal','Sensor pedestal',#15099,#15042);
#15056=PRODUCT_DEFINITION('Load cell envelope','Load cell envelope',#15100,
#15042);
#15057=PRODUCT_DEFINITION('Protective frame','Protective frame',#15101,
#15042);
#15058=PRODUCT_DEFINITION('Foot pad','Foot pad',#15102,#15042);
#15059=PRODUCT_DEFINITION('Foot pad (1)','Foot pad (1)',#15103,#15042);
#15060=PRODUCT_DEFINITION('M6x18 mounting screw','M6x18 mounting screw',
#15104,#15042);
#15061=PRODUCT_DEFINITION('Sealed Ball Bearing - 12 x 32 x 10 mm',
'Sealed Ball Bearing - 12 x 32 x 10 mm',#15105,#15042);
#15062=PRODUCT_DEFINITION('Inner ring','Inner ring',#15106,#15042);
#15063=PRODUCT_DEFINITION('Outer ring','Outer ring',#15107,#15042);
#15064=PRODUCT_DEFINITION('Balls','Balls',#15108,#15042);
#15065=PRODUCT_DEFINITION('Cage','Cage',#15109,#15042);
#15066=PRODUCT_DEFINITION('Seals 2RS','Seals 2RS',#15110,#15042);
#15067=PRODUCT_DEFINITION('Sealed Ball Bearing - 20 x 47 x 14 mm',
'Sealed Ball Bearing - 20 x 47 x 14 mm',#15111,#15042);
#15068=PRODUCT_DEFINITION('Inner ring (1)','Inner ring (1)',#15112,#15042);
#15069=PRODUCT_DEFINITION('Outer ring (1)','Outer ring (1)',#15113,#15042);
#15070=PRODUCT_DEFINITION('Balls (1)','Balls (1)',#15114,#15042);
#15071=PRODUCT_DEFINITION('Cage (1)','Cage (1)',#15115,#15042);
#15072=PRODUCT_DEFINITION('Seals 2RS (1)','Seals 2RS (1)',#15116,#15042);
#15073=PRODUCT_DEFINITION('Cap Screw - M5x20','Cap Screw - M5x20',#15117,
#15042);
#15074=PRODUCT_DEFINITION('M4x10 Cap Screw','M4x10 Cap Screw',#15118,#15042);
#15075=PRODUCT_DEFINITION('Test arbor and drive flange',
'Test arbor and drive flange',#15119,#15042);
#15076=PRODUCT_DEFINITION('Stepped arbor','Stepped arbor',#15120,#15042);
#15077=PRODUCT_DEFINITION('Support inner spacer','Support inner spacer',
#15121,#15042);
#15078=PRODUCT_DEFINITION('Support inner spacer (1)',
'Support inner spacer (1)',#15122,#15042);
#15079=PRODUCT_DEFINITION('Journal collar','Journal collar',#15123,#15042);
#15080=PRODUCT_DEFINITION('Journal collar (1)','Journal collar (1)',#15124,
#15042);
#15081=PRODUCT_DEFINITION('Outer journal spacer','Outer journal spacer',
#15125,#15042);
#15082=PRODUCT_DEFINITION('Outer journal spacer (1)',
'Outer journal spacer (1)',#15126,#15042);
#15083=PRODUCT_DEFINITION('Test bearing collar','Test bearing collar',#15127,
#15042);
#15084=PRODUCT_DEFINITION('Test bearing collar (1)',
'Test bearing collar (1)',#15128,#15042);
#15085=PRODUCT_DEFINITION('Drive flange','Drive flange',#15129,#15042);
#15086=PRODUCT_DEFINITION('Socket Set Screw - M5x8',
'Socket Set Screw - M5x8',#15130,#15042);
#15087=PRODUCT_DEFINITION_FORMATION('',$,#15178);
#15088=PRODUCT_DEFINITION_FORMATION('',$,#15179);
#15089=PRODUCT_DEFINITION_FORMATION('',$,#15180);
#15090=PRODUCT_DEFINITION_FORMATION('',$,#15181);
#15091=PRODUCT_DEFINITION_FORMATION('',$,#15182);
#15092=PRODUCT_DEFINITION_FORMATION('',$,#15183);
#15093=PRODUCT_DEFINITION_FORMATION('',$,#15184);
#15094=PRODUCT_DEFINITION_FORMATION('',$,#15185);
#15095=PRODUCT_DEFINITION_FORMATION('',$,#15186);
#15096=PRODUCT_DEFINITION_FORMATION('',$,#15187);
#15097=PRODUCT_DEFINITION_FORMATION('',$,#15188);
#15098=PRODUCT_DEFINITION_FORMATION('',$,#15189);
#15099=PRODUCT_DEFINITION_FORMATION('',$,#15190);
#15100=PRODUCT_DEFINITION_FORMATION('',$,#15191);
#15101=PRODUCT_DEFINITION_FORMATION('',$,#15192);
#15102=PRODUCT_DEFINITION_FORMATION('',$,#15193);
#15103=PRODUCT_DEFINITION_FORMATION('',$,#15194);
#15104=PRODUCT_DEFINITION_FORMATION('',$,#15195);
#15105=PRODUCT_DEFINITION_FORMATION('',$,#15196);
#15106=PRODUCT_DEFINITION_FORMATION('',$,#15197);
#15107=PRODUCT_DEFINITION_FORMATION('',$,#15198);
#15108=PRODUCT_DEFINITION_FORMATION('',$,#15199);
#15109=PRODUCT_DEFINITION_FORMATION('',$,#15200);
#15110=PRODUCT_DEFINITION_FORMATION('',$,#15201);
#15111=PRODUCT_DEFINITION_FORMATION('',$,#15202);
#15112=PRODUCT_DEFINITION_FORMATION('',$,#15203);
#15113=PRODUCT_DEFINITION_FORMATION('',$,#15204);
#15114=PRODUCT_DEFINITION_FORMATION('',$,#15205);
#15115=PRODUCT_DEFINITION_FORMATION('',$,#15206);
#15116=PRODUCT_DEFINITION_FORMATION('',$,#15207);
#15117=PRODUCT_DEFINITION_FORMATION('',$,#15208);
#15118=PRODUCT_DEFINITION_FORMATION('',$,#15209);
#15119=PRODUCT_DEFINITION_FORMATION('',$,#15210);
#15120=PRODUCT_DEFINITION_FORMATION('',$,#15211);
#15121=PRODUCT_DEFINITION_FORMATION('',$,#15212);
#15122=PRODUCT_DEFINITION_FORMATION('',$,#15213);
#15123=PRODUCT_DEFINITION_FORMATION('',$,#15214);
#15124=PRODUCT_DEFINITION_FORMATION('',$,#15215);
#15125=PRODUCT_DEFINITION_FORMATION('',$,#15216);
#15126=PRODUCT_DEFINITION_FORMATION('',$,#15217);
#15127=PRODUCT_DEFINITION_FORMATION('',$,#15218);
#15128=PRODUCT_DEFINITION_FORMATION('',$,#15219);
#15129=PRODUCT_DEFINITION_FORMATION('',$,#15220);
#15130=PRODUCT_DEFINITION_FORMATION('',$,#15221);
#15131=PRODUCT_RELATED_PRODUCT_CATEGORY('PAT-007','PAT-007',(#15178));
#15132=PRODUCT_RELATED_PRODUCT_CATEGORY('Supports and reaction sensor',
'Supports and reaction sensor',(#15179));
#15133=PRODUCT_RELATED_PRODUCT_CATEGORY('Base','Base',(#15180));
#15134=PRODUCT_RELATED_PRODUCT_CATEGORY('Support housing',
'Support housing',(#15181));
#15135=PRODUCT_RELATED_PRODUCT_CATEGORY('Support cap','Support cap',(#15182));
#15136=PRODUCT_RELATED_PRODUCT_CATEGORY('Support cap (1)',
'Support cap (1)',(#15183));
#15137=PRODUCT_RELATED_PRODUCT_CATEGORY('Support housing (1)',
'Support housing (1)',(#15184));
#15138=PRODUCT_RELATED_PRODUCT_CATEGORY('Support cap (2)',
'Support cap (2)',(#15185));
#15139=PRODUCT_RELATED_PRODUCT_CATEGORY('Support cap (3)',
'Support cap (3)',(#15186));
#15140=PRODUCT_RELATED_PRODUCT_CATEGORY('Reaction housing and arm',
'Reaction housing and arm',(#15187));
#15141=PRODUCT_RELATED_PRODUCT_CATEGORY('Test bearing cap',
'Test bearing cap',(#15188));
#15142=PRODUCT_RELATED_PRODUCT_CATEGORY('Test bearing cap (1)',
'Test bearing cap (1)',(#15189));
#15143=PRODUCT_RELATED_PRODUCT_CATEGORY('Sensor pedestal',
'Sensor pedestal',(#15190));
#15144=PRODUCT_RELATED_PRODUCT_CATEGORY('Load cell envelope',
'Load cell envelope',(#15191));
#15145=PRODUCT_RELATED_PRODUCT_CATEGORY('Protective frame',
'Protective frame',(#15192));
#15146=PRODUCT_RELATED_PRODUCT_CATEGORY('Foot pad','Foot pad',(#15193));
#15147=PRODUCT_RELATED_PRODUCT_CATEGORY('Foot pad (1)','Foot pad (1)',(#15194));
#15148=PRODUCT_RELATED_PRODUCT_CATEGORY('M6x18 mounting screw',
'M6x18 mounting screw',(#15195));
#15149=PRODUCT_RELATED_PRODUCT_CATEGORY(
'Sealed Ball Bearing - 12 x 32 x 10 mm',
'Sealed Ball Bearing - 12 x 32 x 10 mm',(#15196));
#15150=PRODUCT_RELATED_PRODUCT_CATEGORY('Inner ring','Inner ring',(#15197));
#15151=PRODUCT_RELATED_PRODUCT_CATEGORY('Outer ring','Outer ring',(#15198));
#15152=PRODUCT_RELATED_PRODUCT_CATEGORY('Balls','Balls',(#15199));
#15153=PRODUCT_RELATED_PRODUCT_CATEGORY('Cage','Cage',(#15200));
#15154=PRODUCT_RELATED_PRODUCT_CATEGORY('Seals 2RS','Seals 2RS',(#15201));
#15155=PRODUCT_RELATED_PRODUCT_CATEGORY(
'Sealed Ball Bearing - 20 x 47 x 14 mm',
'Sealed Ball Bearing - 20 x 47 x 14 mm',(#15202));
#15156=PRODUCT_RELATED_PRODUCT_CATEGORY('Inner ring (1)',
'Inner ring (1)',(#15203));
#15157=PRODUCT_RELATED_PRODUCT_CATEGORY('Outer ring (1)',
'Outer ring (1)',(#15204));
#15158=PRODUCT_RELATED_PRODUCT_CATEGORY('Balls (1)','Balls (1)',(#15205));
#15159=PRODUCT_RELATED_PRODUCT_CATEGORY('Cage (1)','Cage (1)',(#15206));
#15160=PRODUCT_RELATED_PRODUCT_CATEGORY('Seals 2RS (1)','Seals 2RS (1)',
(#15207));
#15161=PRODUCT_RELATED_PRODUCT_CATEGORY('Cap Screw - M5x20',
'Cap Screw - M5x20',(#15208));
#15162=PRODUCT_RELATED_PRODUCT_CATEGORY('M4x10 Cap Screw',
'M4x10 Cap Screw',(#15209));
#15163=PRODUCT_RELATED_PRODUCT_CATEGORY('Test arbor and drive flange',
'Test arbor and drive flange',(#15210));
#15164=PRODUCT_RELATED_PRODUCT_CATEGORY('Stepped arbor','Stepped arbor',
(#15211));
#15165=PRODUCT_RELATED_PRODUCT_CATEGORY('Support inner spacer',
'Support inner spacer',(#15212));
#15166=PRODUCT_RELATED_PRODUCT_CATEGORY('Support inner spacer (1)',
'Support inner spacer (1)',(#15213));
#15167=PRODUCT_RELATED_PRODUCT_CATEGORY('Journal collar',
'Journal collar',(#15214));
#15168=PRODUCT_RELATED_PRODUCT_CATEGORY('Journal collar (1)',
'Journal collar (1)',(#15215));
#15169=PRODUCT_RELATED_PRODUCT_CATEGORY('Outer journal spacer',
'Outer journal spacer',(#15216));
#15170=PRODUCT_RELATED_PRODUCT_CATEGORY('Outer journal spacer (1)',
'Outer journal spacer (1)',(#15217));
#15171=PRODUCT_RELATED_PRODUCT_CATEGORY('Test bearing collar',
'Test bearing collar',(#15218));
#15172=PRODUCT_RELATED_PRODUCT_CATEGORY('Test bearing collar (1)',
'Test bearing collar (1)',(#15219));
#15173=PRODUCT_RELATED_PRODUCT_CATEGORY('Drive flange','Drive flange',(#15220));
#15174=PRODUCT_RELATED_PRODUCT_CATEGORY('Socket Set Screw - M5x8',
'Socket Set Screw - M5x8',(#15221));
#15175=APPLICATION_PROTOCOL_DEFINITION('international standard',
'automotive_design',2009,#15176);
#15176=APPLICATION_CONTEXT(
'Core Data for Automotive Mechanical Design Process');
#15177=PRODUCT_CONTEXT('part definition',#15176,'mechanical');
#15178=PRODUCT('PAT-007','PAT-007',
'PAT-007',(#15177));
#15179=PRODUCT('Supports and reaction sensor',
'Supports and reaction sensor','Supports and reaction sensor',(#15177));
#15180=PRODUCT('Base','Base','Base',(#15177));
#15181=PRODUCT('Support housing','Support housing','Support housing',(#15177));
#15182=PRODUCT('Support cap','Support cap','Support cap',(#15177));
#15183=PRODUCT('Support cap (1)','Support cap (1)','Support cap (1)',(#15177));
#15184=PRODUCT('Support housing (1)','Support housing (1)',
'Support housing (1)',(#15177));
#15185=PRODUCT('Support cap (2)','Support cap (2)','Support cap (2)',(#15177));
#15186=PRODUCT('Support cap (3)','Support cap (3)','Support cap (3)',(#15177));
#15187=PRODUCT('Reaction housing and arm','Reaction housing and arm',
'Reaction housing and arm',(#15177));
#15188=PRODUCT('Test bearing cap','Test bearing cap','Test bearing cap',
(#15177));
#15189=PRODUCT('Test bearing cap (1)','Test bearing cap (1)',
'Test bearing cap (1)',(#15177));
#15190=PRODUCT('Sensor pedestal','Sensor pedestal','Sensor pedestal',(#15177));
#15191=PRODUCT('Load cell envelope','Load cell envelope',
'Load cell envelope',(#15177));
#15192=PRODUCT('Protective frame','Protective frame','Protective frame',
(#15177));
#15193=PRODUCT('Foot pad','Foot pad','Foot pad',(#15177));
#15194=PRODUCT('Foot pad (1)','Foot pad (1)','Foot pad (1)',(#15177));
#15195=PRODUCT('M6x18 mounting screw','M6x18 mounting screw',
'M6x18 mounting screw',(#15177));
#15196=PRODUCT('Sealed Ball Bearing - 12 x 32 x 10 mm',
'Sealed Ball Bearing - 12 x 32 x 10 mm',
'Sealed Ball Bearing - 12 x 32 x 10 mm',(#15177));
#15197=PRODUCT('Inner ring','Inner ring','Inner ring',(#15177));
#15198=PRODUCT('Outer ring','Outer ring','Outer ring',(#15177));
#15199=PRODUCT('Balls','Balls','Balls',(#15177));
#15200=PRODUCT('Cage','Cage','Cage',(#15177));
#15201=PRODUCT('Seals 2RS','Seals 2RS','Seals 2RS',(#15177));
#15202=PRODUCT('Sealed Ball Bearing - 20 x 47 x 14 mm',
'Sealed Ball Bearing - 20 x 47 x 14 mm',
'Sealed Ball Bearing - 20 x 47 x 14 mm',(#15177));
#15203=PRODUCT('Inner ring (1)','Inner ring (1)','Inner ring (1)',(#15177));
#15204=PRODUCT('Outer ring (1)','Outer ring (1)','Outer ring (1)',(#15177));
#15205=PRODUCT('Balls (1)','Balls (1)','Balls (1)',(#15177));
#15206=PRODUCT('Cage (1)','Cage (1)','Cage (1)',(#15177));
#15207=PRODUCT('Seals 2RS (1)','Seals 2RS (1)','Seals 2RS (1)',(#15177));
#15208=PRODUCT('Cap Screw - M5x20','Cap Screw - M5x20',
'Cap Screw - M5x20',(#15177));
#15209=PRODUCT('M4x10 Cap Screw','M4x10 Cap Screw','M4x10 Cap Screw',(#15177));
#15210=PRODUCT('Test arbor and drive flange',
'Test arbor and drive flange','Test arbor and drive flange',(#15177));
#15211=PRODUCT('Stepped arbor','Stepped arbor','Stepped arbor',(#15177));
#15212=PRODUCT('Support inner spacer','Support inner spacer',
'Support inner spacer',(#15177));
#15213=PRODUCT('Support inner spacer (1)','Support inner spacer (1)',
'Support inner spacer (1)',(#15177));
#15214=PRODUCT('Journal collar','Journal collar','Journal collar',(#15177));
#15215=PRODUCT('Journal collar (1)','Journal collar (1)','Journal collar (1)',
(#15177));
#15216=PRODUCT('Outer journal spacer','Outer journal spacer',
'Outer journal spacer',(#15177));
#15217=PRODUCT('Outer journal spacer (1)','Outer journal spacer (1)',
'Outer journal spacer (1)',(#15177));
#15218=PRODUCT('Test bearing collar','Test bearing collar',
'Test bearing collar',(#15177));
#15219=PRODUCT('Test bearing collar (1)','Test bearing collar (1)',
'Test bearing collar (1)',(#15177));
#15220=PRODUCT('Drive flange','Drive flange','Drive flange',(#15177));
#15221=PRODUCT('Socket Set Screw - M5x8','Socket Set Screw - M5x8',
'Socket Set Screw - M5x8',(#15177));
#15222=PRESENTATION_STYLE_ASSIGNMENT((#15227));
#15223=PRESENTATION_STYLE_ASSIGNMENT((#15228));
#15224=PRESENTATION_STYLE_ASSIGNMENT((#15229));
#15225=PRESENTATION_STYLE_ASSIGNMENT((#15230));
#15226=PRESENTATION_STYLE_ASSIGNMENT((#15231));
#15227=SURFACE_STYLE_USAGE(.BOTH.,#15232);
#15228=SURFACE_STYLE_USAGE(.BOTH.,#15233);
#15229=SURFACE_STYLE_USAGE(.BOTH.,#15234);
#15230=SURFACE_STYLE_USAGE(.BOTH.,#15235);
#15231=SURFACE_STYLE_USAGE(.BOTH.,#15236);
#15232=SURFACE_SIDE_STYLE('',(#15237));
#15233=SURFACE_SIDE_STYLE('',(#15238));
#15234=SURFACE_SIDE_STYLE('',(#15239));
#15235=SURFACE_SIDE_STYLE('',(#15240));
#15236=SURFACE_SIDE_STYLE('',(#15241));
#15237=SURFACE_STYLE_FILL_AREA(#15242);
#15238=SURFACE_STYLE_FILL_AREA(#15243);
#15239=SURFACE_STYLE_FILL_AREA(#15244);
#15240=SURFACE_STYLE_FILL_AREA(#15245);
#15241=SURFACE_STYLE_FILL_AREA(#15246);
#15242=FILL_AREA_STYLE('Steel - Satin',(#15247));
#15243=FILL_AREA_STYLE('CAD Library Painted - Deep blue',(#15248));
#15244=FILL_AREA_STYLE('CAD Library Painted - Engineering blue',(#15249));
#15245=FILL_AREA_STYLE('CAD Library Painted - Steel gray',(#15250));
#15246=FILL_AREA_STYLE('CAD Library Painted - Graphite',(#15251));
#15247=FILL_AREA_STYLE_COLOUR('Steel - Satin',#15252);
#15248=FILL_AREA_STYLE_COLOUR('CAD Library Painted - Deep blue',#15253);
#15249=FILL_AREA_STYLE_COLOUR('CAD Library Painted - Engineering blue',
#15254);
#15250=FILL_AREA_STYLE_COLOUR('CAD Library Painted - Steel gray',#15255);
#15251=FILL_AREA_STYLE_COLOUR('CAD Library Painted - Graphite',#15256);
#15252=COLOUR_RGB('Steel - Satin',0.627450980392157,0.627450980392157,0.627450980392157);
#15253=COLOUR_RGB('CAD Library Painted - Deep blue',0.0784313725490196,
0.203921568627451,0.349019607843137);
#15254=COLOUR_RGB('CAD Library Painted - Engineering blue',0.12156862745098,
0.356862745098039,0.6);
#15255=COLOUR_RGB('CAD Library Painted - Steel gray',0.592156862745098,
0.631372549019608,0.67843137254902);
#15256=COLOUR_RGB('CAD Library Painted - Graphite',0.168627450980392,0.192156862745098,
0.231372549019608);
#15257=COLOUR_RGB('Dark Blue',0.08,0.2,0.34);
#15258=FILL_AREA_STYLE_COLOUR('',#15257);
#15259=FILL_AREA_STYLE('',(#15258));
#15260=SURFACE_STYLE_FILL_AREA(#15259);
#15261=SURFACE_SIDE_STYLE('',(#15260));
#15262=SURFACE_STYLE_USAGE(.BOTH.,#15261);
#15263=PRESENTATION_STYLE_ASSIGNMENT((#15262));
#15264=COLOUR_RGB('Light Blue',0.38,0.62,0.78);
#15265=FILL_AREA_STYLE_COLOUR('',#15264);
#15266=FILL_AREA_STYLE('',(#15265));
#15267=SURFACE_STYLE_FILL_AREA(#15266);
#15268=SURFACE_SIDE_STYLE('',(#15267));
#15269=SURFACE_STYLE_USAGE(.BOTH.,#15268);
#15270=PRESENTATION_STYLE_ASSIGNMENT((#15269));
#15271=COLOUR_RGB('Sky Blue',0.24,0.69,0.87);
#15272=FILL_AREA_STYLE_COLOUR('',#15271);
#15273=FILL_AREA_STYLE('',(#15272));
#15274=SURFACE_STYLE_FILL_AREA(#15273);
#15275=SURFACE_SIDE_STYLE('',(#15274));
#15276=SURFACE_STYLE_USAGE(.BOTH.,#15275);
#15277=PRESENTATION_STYLE_ASSIGNMENT((#15276));
#15278=COLOUR_RGB('Grey',0.48,0.52,0.57);
#15279=FILL_AREA_STYLE_COLOUR('',#15278);
#15280=FILL_AREA_STYLE('',(#15279));
#15281=SURFACE_STYLE_FILL_AREA(#15280);
#15282=SURFACE_SIDE_STYLE('',(#15281));
#15283=SURFACE_STYLE_USAGE(.BOTH.,#15282);
#15284=PRESENTATION_STYLE_ASSIGNMENT((#15283));
#15285=COLOUR_RGB('Black',0.12,0.14,0.17);
#15286=FILL_AREA_STYLE_COLOUR('',#15285);
#15287=FILL_AREA_STYLE('',(#15286));
#15288=SURFACE_STYLE_FILL_AREA(#15287);
#15289=SURFACE_SIDE_STYLE('',(#15288));
#15290=SURFACE_STYLE_USAGE(.BOTH.,#15289);
#15291=PRESENTATION_STYLE_ASSIGNMENT((#15290));
#15292=COLOUR_RGB('Off White',0.89,0.88,0.83);
#15293=FILL_AREA_STYLE_COLOUR('',#15292);
#15294=FILL_AREA_STYLE('',(#15293));
#15295=SURFACE_STYLE_FILL_AREA(#15294);
#15296=SURFACE_SIDE_STYLE('',(#15295));
#15297=SURFACE_STYLE_USAGE(.BOTH.,#15296);
#15298=PRESENTATION_STYLE_ASSIGNMENT((#15297));
ENDSEC;
END-ISO-10303-21;
